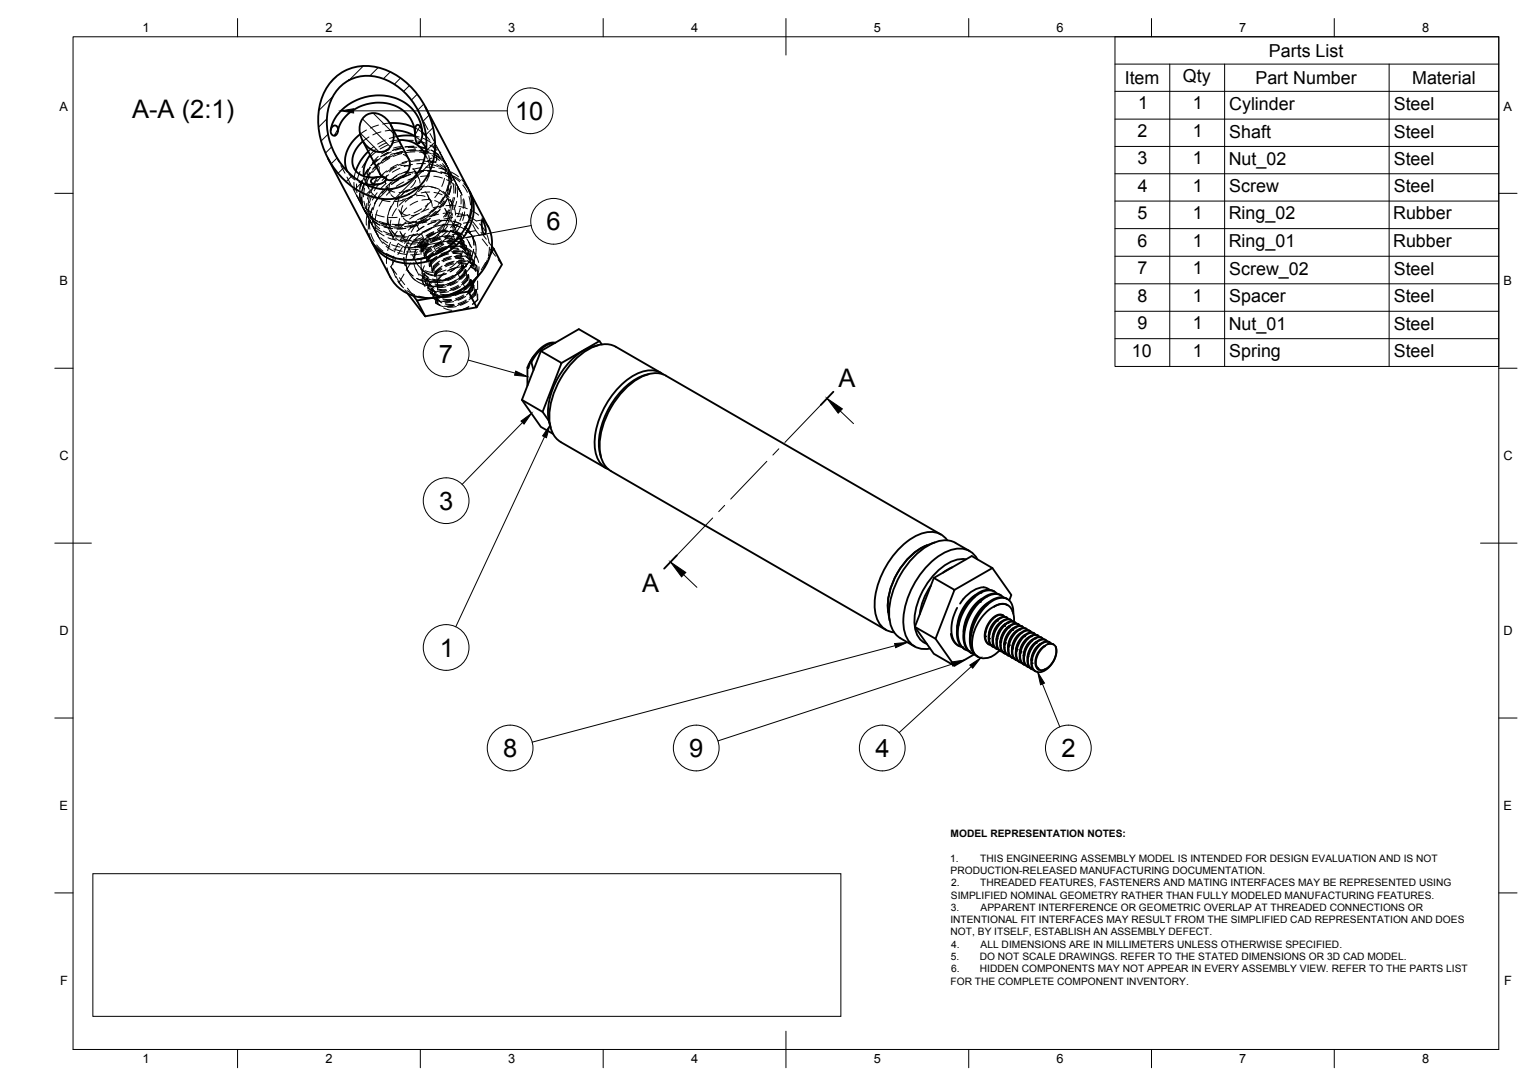
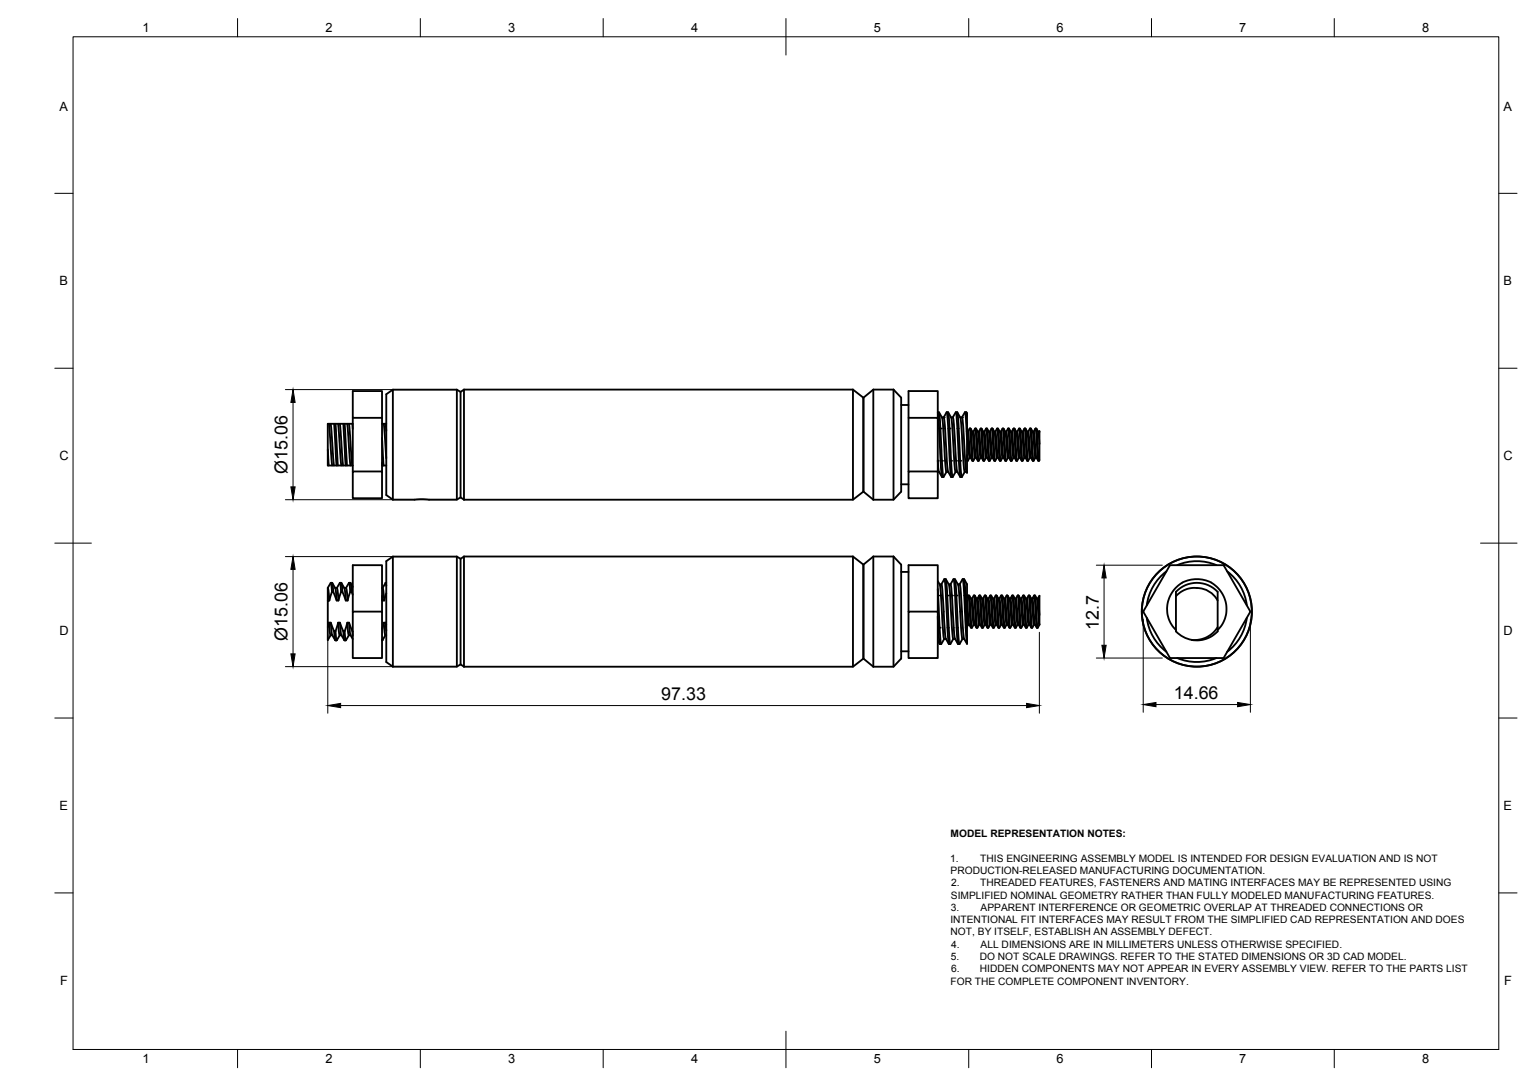
ISO-10303-21;
HEADER;
/* Generated by software containing ST-Developer
 * from STEP Tools, Inc. (www.steptools.com) 
 */

FILE_DESCRIPTION(
/* description */ (''),
/* implementation_level */ '2;1');

FILE_NAME(
/* name */ 'BR-313',
/* time_stamp */ '2026-10-06T13:05:37-07:00',
/* author */ (''),
/* organization */ (''),
/* preprocessor_version */ 'ST-DEVELOPER v20.2',
/* originating_system */ 'Autodesk Translation Framework v15.15.0.0',
/* authorisation */ '');

FILE_SCHEMA (('AUTOMOTIVE_DESIGN { 1 0 10303 214 3 1 1 }'));
ENDSEC;

DATA;
#10=MECHANICAL_DESIGN_GEOMETRIC_PRESENTATION_REPRESENTATION('',(#136,#137,
#138,#139,#140,#141,#142,#143,#144,#145),#28055);
#11=ITEM_DEFINED_TRANSFORMATION($,$,#3801,#4104);
#12=ITEM_DEFINED_TRANSFORMATION($,$,#3851,#4105);
#13=ITEM_DEFINED_TRANSFORMATION($,$,#3947,#4106);
#14=ITEM_DEFINED_TRANSFORMATION($,$,#3962,#4107);
#15=ITEM_DEFINED_TRANSFORMATION($,$,#3990,#4108);
#16=ITEM_DEFINED_TRANSFORMATION($,$,#4002,#4109);
#17=ITEM_DEFINED_TRANSFORMATION($,$,#4014,#4110);
#18=ITEM_DEFINED_TRANSFORMATION($,$,#4059,#4111);
#19=ITEM_DEFINED_TRANSFORMATION($,$,#4086,#4112);
#20=ITEM_DEFINED_TRANSFORMATION($,$,#4101,#4113);
#21=(
REPRESENTATION_RELATIONSHIP($,$,#28093,#28092)
REPRESENTATION_RELATIONSHIP_WITH_TRANSFORMATION(#11)
SHAPE_REPRESENTATION_RELATIONSHIP()
);
#22=(
REPRESENTATION_RELATIONSHIP($,$,#28094,#28092)
REPRESENTATION_RELATIONSHIP_WITH_TRANSFORMATION(#12)
SHAPE_REPRESENTATION_RELATIONSHIP()
);
#23=(
REPRESENTATION_RELATIONSHIP($,$,#28095,#28092)
REPRESENTATION_RELATIONSHIP_WITH_TRANSFORMATION(#13)
SHAPE_REPRESENTATION_RELATIONSHIP()
);
#24=(
REPRESENTATION_RELATIONSHIP($,$,#28096,#28092)
REPRESENTATION_RELATIONSHIP_WITH_TRANSFORMATION(#14)
SHAPE_REPRESENTATION_RELATIONSHIP()
);
#25=(
REPRESENTATION_RELATIONSHIP($,$,#28097,#28092)
REPRESENTATION_RELATIONSHIP_WITH_TRANSFORMATION(#15)
SHAPE_REPRESENTATION_RELATIONSHIP()
);
#26=(
REPRESENTATION_RELATIONSHIP($,$,#28098,#28092)
REPRESENTATION_RELATIONSHIP_WITH_TRANSFORMATION(#16)
SHAPE_REPRESENTATION_RELATIONSHIP()
);
#27=(
REPRESENTATION_RELATIONSHIP($,$,#28099,#28092)
REPRESENTATION_RELATIONSHIP_WITH_TRANSFORMATION(#17)
SHAPE_REPRESENTATION_RELATIONSHIP()
);
#28=(
REPRESENTATION_RELATIONSHIP($,$,#28100,#28092)
REPRESENTATION_RELATIONSHIP_WITH_TRANSFORMATION(#18)
SHAPE_REPRESENTATION_RELATIONSHIP()
);
#29=(
REPRESENTATION_RELATIONSHIP($,$,#28101,#28092)
REPRESENTATION_RELATIONSHIP_WITH_TRANSFORMATION(#19)
SHAPE_REPRESENTATION_RELATIONSHIP()
);
#30=(
REPRESENTATION_RELATIONSHIP($,$,#28102,#28092)
REPRESENTATION_RELATIONSHIP_WITH_TRANSFORMATION(#20)
SHAPE_REPRESENTATION_RELATIONSHIP()
);
#31=CONTEXT_DEPENDENT_SHAPE_REPRESENTATION(#21,#28082);
#32=CONTEXT_DEPENDENT_SHAPE_REPRESENTATION(#22,#28083);
#33=CONTEXT_DEPENDENT_SHAPE_REPRESENTATION(#23,#28084);
#34=CONTEXT_DEPENDENT_SHAPE_REPRESENTATION(#24,#28085);
#35=CONTEXT_DEPENDENT_SHAPE_REPRESENTATION(#25,#28086);
#36=CONTEXT_DEPENDENT_SHAPE_REPRESENTATION(#26,#28087);
#37=CONTEXT_DEPENDENT_SHAPE_REPRESENTATION(#27,#28088);
#38=CONTEXT_DEPENDENT_SHAPE_REPRESENTATION(#28,#28089);
#39=CONTEXT_DEPENDENT_SHAPE_REPRESENTATION(#29,#28090);
#40=CONTEXT_DEPENDENT_SHAPE_REPRESENTATION(#30,#28091);
#41=NEXT_ASSEMBLY_USAGE_OCCURRENCE('Cylinder:1','Cylinder:1',
'Cylinder:1',#28104,#28105,'Cylinder:1');
#42=NEXT_ASSEMBLY_USAGE_OCCURRENCE('Shaft:1','Shaft:1','Shaft:1',#28104,
#28106,'Shaft:1');
#43=NEXT_ASSEMBLY_USAGE_OCCURRENCE('Nut_02:1','Nut_02:1','Nut_02:1',#28104,
#28107,'Nut_02:1');
#44=NEXT_ASSEMBLY_USAGE_OCCURRENCE('Screw:1','Screw:1','Screw:1',#28104,
#28108,'Screw:1');
#45=NEXT_ASSEMBLY_USAGE_OCCURRENCE('Ring_02:1','Ring_02:1','Ring_02:1',
#28104,#28109,'Ring_02:1');
#46=NEXT_ASSEMBLY_USAGE_OCCURRENCE('Ring_01:1','Ring_01:1','Ring_01:1',
#28104,#28110,'Ring_01:1');
#47=NEXT_ASSEMBLY_USAGE_OCCURRENCE('Screw_02:1','Screw_02:1',
'Screw_02:1',#28104,#28111,'Screw_02:1');
#48=NEXT_ASSEMBLY_USAGE_OCCURRENCE('Spacer:1','Spacer:1','Spacer:1',#28104,
#28112,'Spacer:1');
#49=NEXT_ASSEMBLY_USAGE_OCCURRENCE('Nut_01:1','Nut_01:1','Nut_01:1',#28104,
#28113,'Nut_01:1');
#50=NEXT_ASSEMBLY_USAGE_OCCURRENCE('Spring:1','Spring:1','Spring:1',#28104,
#28114,'Spring:1');
#51=ORIENTED_CLOSED_SHELL('',*,#3684,.F.);
#52=ORIENTED_CLOSED_SHELL('',*,#3685,.F.);
#53=BREP_WITH_VOIDS('Body1',#3686,(#51,#52));
#54=ELLIPSE('',#4033,3.36109563026061,2.90329889035631);
#55=ELLIPSE('',#4034,2.84121050972126,2.43735261139454);
#56=ELLIPSE('',#4052,3.33206993022602,2.82346550068506);
#57=ELLIPSE('',#4053,2.87565474083181,2.48077736727696);
#58=B_SPLINE_SURFACE_WITH_KNOTS('',3,3,((#14364,#14365,#14366,#14367,#14368,
#14369,#14370,#14371,#14372,#14373,#14374,#14375,#14376,#14377,#14378,#14379,
#14380,#14381,#14382,#14383,#14384,#14385,#14386,#14387,#14388,#14389,#14390,
#14391,#14392,#14393,#14394,#14395,#14396,#14397,#14398,#14399,#14400,#14401,
#14402,#14403,#14404,#14405,#14406,#14407,#14408,#14409,#14410,#14411,#14412,
#14413,#14414,#14415,#14416,#14417,#14418,#14419,#14420,#14421,#14422,#14423,
#14424,#14425,#14426,#14427,#14428,#14429,#14430,#14431,#14432,#14433,#14434,
#14435,#14436,#14437,#14438,#14439,#14440,#14441,#14442,#14443,#14444,#14445,
#14446,#14447,#14448,#14449,#14450,#14451,#14452),(#14453,#14454,#14455,
#14456,#14457,#14458,#14459,#14460,#14461,#14462,#14463,#14464,#14465,#14466,
#14467,#14468,#14469,#14470,#14471,#14472,#14473,#14474,#14475,#14476,#14477,
#14478,#14479,#14480,#14481,#14482,#14483,#14484,#14485,#14486,#14487,#14488,
#14489,#14490,#14491,#14492,#14493,#14494,#14495,#14496,#14497,#14498,#14499,
#14500,#14501,#14502,#14503,#14504,#14505,#14506,#14507,#14508,#14509,#14510,
#14511,#14512,#14513,#14514,#14515,#14516,#14517,#14518,#14519,#14520,#14521,
#14522,#14523,#14524,#14525,#14526,#14527,#14528,#14529,#14530,#14531,#14532,
#14533,#14534,#14535,#14536,#14537,#14538,#14539,#14540,#14541),(#14542,
#14543,#14544,#14545,#14546,#14547,#14548,#14549,#14550,#14551,#14552,#14553,
#14554,#14555,#14556,#14557,#14558,#14559,#14560,#14561,#14562,#14563,#14564,
#14565,#14566,#14567,#14568,#14569,#14570,#14571,#14572,#14573,#14574,#14575,
#14576,#14577,#14578,#14579,#14580,#14581,#14582,#14583,#14584,#14585,#14586,
#14587,#14588,#14589,#14590,#14591,#14592,#14593,#14594,#14595,#14596,#14597,
#14598,#14599,#14600,#14601,#14602,#14603,#14604,#14605,#14606,#14607,#14608,
#14609,#14610,#14611,#14612,#14613,#14614,#14615,#14616,#14617,#14618,#14619,
#14620,#14621,#14622,#14623,#14624,#14625,#14626,#14627,#14628,#14629,#14630),
(#14631,#14632,#14633,#14634,#14635,#14636,#14637,#14638,#14639,#14640,
#14641,#14642,#14643,#14644,#14645,#14646,#14647,#14648,#14649,#14650,#14651,
#14652,#14653,#14654,#14655,#14656,#14657,#14658,#14659,#14660,#14661,#14662,
#14663,#14664,#14665,#14666,#14667,#14668,#14669,#14670,#14671,#14672,#14673,
#14674,#14675,#14676,#14677,#14678,#14679,#14680,#14681,#14682,#14683,#14684,
#14685,#14686,#14687,#14688,#14689,#14690,#14691,#14692,#14693,#14694,#14695,
#14696,#14697,#14698,#14699,#14700,#14701,#14702,#14703,#14704,#14705,#14706,
#14707,#14708,#14709,#14710,#14711,#14712,#14713,#14714,#14715,#14716,#14717,
#14718,#14719)),.UNSPECIFIED.,.F.,.F.,.F.,(4,4),(4,1,1,1,1,1,1,1,1,1,1,
1,1,1,1,1,1,1,1,1,1,1,1,1,1,1,1,1,1,1,1,1,1,1,1,1,1,1,1,1,1,1,1,1,1,1,1,
1,1,1,1,1,1,1,1,1,1,1,1,1,1,1,1,1,1,1,1,1,1,1,1,1,1,1,1,1,1,1,1,1,1,1,1,
1,1,1,4),(-0.000373179544599254,0.0497114942005783),(13.3942556087771,14.3924503130856,
15.3906450173941,16.3888397217026,17.3870344260111,18.3852291303196,19.3834238346281,
20.3816185389366,21.3798132432451,22.3780079475536,23.3762026518621,24.3743973561706,
25.3725920604791,26.3707867647876,27.3689814690961,28.3671761734046,29.365370877713,
30.3635655820215,31.36176028633,32.3599549906385,33.358149694947,34.3563443992555,
35.354539103564,36.3527338078725,37.350928512181,38.3491232164895,39.347317920798,
40.3455126251065,41.343707329415,42.3419020337235,43.340096738032,44.3382914423405,
45.336486146649,46.3346808509575,47.332875555266,48.3310702595745,49.329264963883,
50.3274596681915,51.3256543725,52.3238490768085,53.322043781117,54.3202384854255,
55.318433189734,56.3166278940425,57.314822598351,58.3130173026595,59.311212006968,
60.3094067112765,61.307601415585,62.3057961198935,63.303990824202,64.3021855285105,
65.300380232819,66.2985749371275,67.296769641436,68.2949643457444,69.2931590500529,
70.2913537543614,71.2895484586699,72.2877431629784,73.2859378672869,74.2841325715954,
75.2823272759039,76.2805219802124,77.2787166845209,78.2769113888294,79.2751060931379,
80.2733007974464,81.2714955017549,82.2696902060634,83.2678849103719,84.2660796146804,
85.2642743189889,86.2624690232974,87.2606637276059,88.2588584319144,89.2570531362229,
90.2552478405314,91.2534425448399,92.2516372491484,93.2498319534569,94.2480266577654,
95.2462213620739,96.2444160663824,97.2426107706909,98.2408054749994,99.2393733588525),
 .UNSPECIFIED.);
#59=B_SPLINE_SURFACE_WITH_KNOTS('',3,3,((#14976,#14977,#14978,#14979,#14980,
#14981,#14982,#14983,#14984,#14985,#14986,#14987,#14988,#14989,#14990,#14991,
#14992,#14993,#14994,#14995,#14996,#14997,#14998,#14999,#15000,#15001,#15002,
#15003,#15004,#15005,#15006,#15007,#15008,#15009,#15010,#15011,#15012,#15013,
#15014,#15015,#15016,#15017,#15018,#15019,#15020,#15021,#15022,#15023,#15024,
#15025,#15026,#15027,#15028,#15029,#15030,#15031,#15032,#15033,#15034,#15035,
#15036,#15037,#15038,#15039,#15040,#15041,#15042,#15043,#15044,#15045,#15046,
#15047,#15048,#15049,#15050,#15051,#15052,#15053,#15054,#15055,#15056,#15057,
#15058,#15059,#15060,#15061,#15062,#15063,#15064),(#15065,#15066,#15067,
#15068,#15069,#15070,#15071,#15072,#15073,#15074,#15075,#15076,#15077,#15078,
#15079,#15080,#15081,#15082,#15083,#15084,#15085,#15086,#15087,#15088,#15089,
#15090,#15091,#15092,#15093,#15094,#15095,#15096,#15097,#15098,#15099,#15100,
#15101,#15102,#15103,#15104,#15105,#15106,#15107,#15108,#15109,#15110,#15111,
#15112,#15113,#15114,#15115,#15116,#15117,#15118,#15119,#15120,#15121,#15122,
#15123,#15124,#15125,#15126,#15127,#15128,#15129,#15130,#15131,#15132,#15133,
#15134,#15135,#15136,#15137,#15138,#15139,#15140,#15141,#15142,#15143,#15144,
#15145,#15146,#15147,#15148,#15149,#15150,#15151,#15152,#15153),(#15154,
#15155,#15156,#15157,#15158,#15159,#15160,#15161,#15162,#15163,#15164,#15165,
#15166,#15167,#15168,#15169,#15170,#15171,#15172,#15173,#15174,#15175,#15176,
#15177,#15178,#15179,#15180,#15181,#15182,#15183,#15184,#15185,#15186,#15187,
#15188,#15189,#15190,#15191,#15192,#15193,#15194,#15195,#15196,#15197,#15198,
#15199,#15200,#15201,#15202,#15203,#15204,#15205,#15206,#15207,#15208,#15209,
#15210,#15211,#15212,#15213,#15214,#15215,#15216,#15217,#15218,#15219,#15220,
#15221,#15222,#15223,#15224,#15225,#15226,#15227,#15228,#15229,#15230,#15231,
#15232,#15233,#15234,#15235,#15236,#15237,#15238,#15239,#15240,#15241,#15242),
(#15243,#15244,#15245,#15246,#15247,#15248,#15249,#15250,#15251,#15252,
#15253,#15254,#15255,#15256,#15257,#15258,#15259,#15260,#15261,#15262,#15263,
#15264,#15265,#15266,#15267,#15268,#15269,#15270,#15271,#15272,#15273,#15274,
#15275,#15276,#15277,#15278,#15279,#15280,#15281,#15282,#15283,#15284,#15285,
#15286,#15287,#15288,#15289,#15290,#15291,#15292,#15293,#15294,#15295,#15296,
#15297,#15298,#15299,#15300,#15301,#15302,#15303,#15304,#15305,#15306,#15307,
#15308,#15309,#15310,#15311,#15312,#15313,#15314,#15315,#15316,#15317,#15318,
#15319,#15320,#15321,#15322,#15323,#15324,#15325,#15326,#15327,#15328,#15329,
#15330,#15331)),.UNSPECIFIED.,.F.,.F.,.F.,(4,4),(4,1,1,1,1,1,1,1,1,1,1,
1,1,1,1,1,1,1,1,1,1,1,1,1,1,1,1,1,1,1,1,1,1,1,1,1,1,1,1,1,1,1,1,1,1,1,1,
1,1,1,1,1,1,1,1,1,1,1,1,1,1,1,1,1,1,1,1,1,1,1,1,1,1,1,1,1,1,1,1,1,1,1,1,
1,1,1,4),(-0.000317322289268298,0.0497654761150975),(16.7016191235447,17.7001869884391,
18.6983816927476,19.6965763970561,20.6947711013646,21.6929658056731,22.6911605099816,
23.6893552142901,24.6875499185986,25.6857446229071,26.6839393272156,27.6821340315241,
28.6803287358326,29.6785234401411,30.6767181444496,31.6749128487581,32.6731075530666,
33.6713022573751,34.6694969616836,35.6676916659921,36.6658863703006,37.6640810746091,
38.6622757789176,39.6604704832261,40.6586651875346,41.6568598918431,42.6550545961516,
43.65324930046,44.6514440047685,45.6496387090771,46.6478334133855,47.646028117694,
48.6442228220025,49.642417526311,50.6406122306195,51.638806934928,52.6370016392365,
53.635196343545,54.6333910478535,55.631585752162,56.6297804564705,57.627975160779,
58.6261698650875,59.624364569396,60.6225592737045,61.620753978013,62.6189486823215,
63.61714338663,64.6153380909385,65.613532795247,66.6117274995555,67.609922203864,
68.6081169081725,69.606311612481,70.6045063167895,71.602701021098,72.6008957254065,
73.599090429715,74.5972851340235,75.595479838332,76.5936745426405,77.591869246949,
78.5900639512575,79.588258655566,80.5864533598745,81.584648064183,82.5828427684915,
83.5810374728,84.5792321771085,85.577426881417,86.5756215857255,87.573816290034,
88.5720109943425,89.570205698651,90.5684004029595,91.566595107268,92.5647898115765,
93.562984515885,94.5611792201935,95.559373924502,96.5575686288105,97.555763333119,
98.5539580374275,99.552152741736,100.550347446044,101.548542150353,102.546736854661),
 .UNSPECIFIED.);
#60=B_SPLINE_SURFACE_WITH_KNOTS('',3,1,((#15514,#15515),(#15516,#15517),
(#15518,#15519),(#15520,#15521),(#15522,#15523),(#15524,#15525),(#15526,
#15527),(#15528,#15529),(#15530,#15531),(#15532,#15533),(#15534,#15535),
(#15536,#15537),(#15538,#15539),(#15540,#15541)),.UNSPECIFIED.,.F.,.F.,
 .F.,(4,2,2,2,2,2,4),(2,2),(-0.844212290556731,-0.730966332817565,-0.619975754240938,
-0.457326579004558,-0.29977928179387,-0.147336283383114,0.),(0.,0.48),
 .UNSPECIFIED.);
#61=B_SPLINE_SURFACE_WITH_KNOTS('',3,1,((#15582,#15583),(#15584,#15585),
(#15586,#15587),(#15588,#15589),(#15590,#15591),(#15592,#15593),(#15594,
#15595),(#15596,#15597),(#15598,#15599),(#15600,#15601),(#15602,#15603),
(#15604,#15605),(#15606,#15607),(#15608,#15609)),.UNSPECIFIED.,.F.,.F.,
 .F.,(4,2,2,2,2,2,4),(2,2),(-0.847325527525843,-0.749719327139836,-0.649860858750851,
-0.495073659399383,-0.335166304629316,-0.170141007879843,0.),(0.,0.48),
 .UNSPECIFIED.);
#62=B_SPLINE_SURFACE_WITH_KNOTS('',3,3,((#20854,#20855,#20856,#20857,#20858,
#20859),(#20860,#20861,#20862,#20863,#20864,#20865),(#20866,#20867,#20868,
#20869,#20870,#20871),(#20872,#20873,#20874,#20875,#20876,#20877)),
 .UNSPECIFIED.,.F.,.F.,.F.,(4,4),(4,1,1,4),(0.,0.0494711118308268),(16.7019134878289,
17.6517088926312,18.6014255011318,19.5511421096324),.UNSPECIFIED.);
#63=B_SPLINE_SURFACE_WITH_KNOTS('',3,3,((#21117,#21118,#21119,#21120,#21121,
#21122),(#21123,#21124,#21125,#21126,#21127,#21128),(#21129,#21130,#21131,
#21132,#21133,#21134),(#21135,#21136,#21137,#21138,#21139,#21140)),
 .UNSPECIFIED.,.F.,.F.,.F.,(4,4),(4,1,1,4),(-7.87913040489834E-5,0.0493923155291723),
(13.3942556087771,14.3439722172777,15.2936888257783,16.2434842255829),
 .UNSPECIFIED.);
#64=B_SPLINE_SURFACE_WITH_KNOTS('',3,3,((#21329,#21330,#21331,#21332,#21333,
#21334,#21335,#21336,#21337,#21338,#21339,#21340,#21341,#21342,#21343,#21344,
#21345,#21346,#21347,#21348,#21349,#21350,#21351,#21352,#21353,#21354,#21355,
#21356,#21357,#21358,#21359,#21360,#21361,#21362,#21363,#21364,#21365,#21366,
#21367,#21368,#21369,#21370,#21371,#21372,#21373,#21374,#21375,#21376),
(#21377,#21378,#21379,#21380,#21381,#21382,#21383,#21384,#21385,#21386,
#21387,#21388,#21389,#21390,#21391,#21392,#21393,#21394,#21395,#21396,#21397,
#21398,#21399,#21400,#21401,#21402,#21403,#21404,#21405,#21406,#21407,#21408,
#21409,#21410,#21411,#21412,#21413,#21414,#21415,#21416,#21417,#21418,#21419,
#21420,#21421,#21422,#21423,#21424),(#21425,#21426,#21427,#21428,#21429,
#21430,#21431,#21432,#21433,#21434,#21435,#21436,#21437,#21438,#21439,#21440,
#21441,#21442,#21443,#21444,#21445,#21446,#21447,#21448,#21449,#21450,#21451,
#21452,#21453,#21454,#21455,#21456,#21457,#21458,#21459,#21460,#21461,#21462,
#21463,#21464,#21465,#21466,#21467,#21468,#21469,#21470,#21471,#21472),
(#21473,#21474,#21475,#21476,#21477,#21478,#21479,#21480,#21481,#21482,
#21483,#21484,#21485,#21486,#21487,#21488,#21489,#21490,#21491,#21492,#21493,
#21494,#21495,#21496,#21497,#21498,#21499,#21500,#21501,#21502,#21503,#21504,
#21505,#21506,#21507,#21508,#21509,#21510,#21511,#21512,#21513,#21514,#21515,
#21516,#21517,#21518,#21519,#21520)),.UNSPECIFIED.,.F.,.F.,.F.,(4,4),(4,
1,1,1,1,1,1,1,1,1,1,1,1,1,1,1,1,1,1,1,1,1,1,1,1,1,1,1,1,1,1,1,1,1,1,1,1,
1,1,1,1,1,1,1,1,4),(-0.000683464176930082,0.0823722747458684),(8.31487785380719,
8.80643119756841,9.29798454132964,10.2810912288521,11.2641979163745,12.247304603897,
13.2304112914194,14.2135179789419,15.1966246664643,16.1797313539867,17.1628380415092,
18.1459447290316,19.1290514165541,20.1121581040765,21.095264791599,22.0783714791214,
23.0614781666439,24.0445848541663,25.0276915416888,26.0107982292112,26.9939049167336,
27.9770116042561,28.9601182917785,29.943224979301,30.9263316668234,31.9094383543459,
32.8925450418683,33.8756517293908,34.8587584169132,35.8418651044356,36.8249717919581,
37.8080784794805,38.791185167003,39.7742918545254,40.7573985420479,41.7405052295703,
42.7236119170928,43.7067186046152,44.6898252921376,45.6729319796601,46.6560386671825,
47.639145354705,48.6222520422274,49.6053587297499,50.0969120735111,50.5891488814492),
 .UNSPECIFIED.);
#65=B_SPLINE_SURFACE_WITH_KNOTS('',3,3,((#21721,#21722,#21723,#21724,#21725,
#21726,#21727,#21728,#21729,#21730,#21731,#21732,#21733,#21734,#21735,#21736,
#21737,#21738,#21739,#21740,#21741,#21742,#21743,#21744,#21745,#21746,#21747,
#21748,#21749,#21750,#21751,#21752,#21753,#21754,#21755,#21756,#21757,#21758,
#21759,#21760,#21761,#21762,#21763,#21764,#21765,#21766,#21767,#21768),
(#21769,#21770,#21771,#21772,#21773,#21774,#21775,#21776,#21777,#21778,
#21779,#21780,#21781,#21782,#21783,#21784,#21785,#21786,#21787,#21788,#21789,
#21790,#21791,#21792,#21793,#21794,#21795,#21796,#21797,#21798,#21799,#21800,
#21801,#21802,#21803,#21804,#21805,#21806,#21807,#21808,#21809,#21810,#21811,
#21812,#21813,#21814,#21815,#21816),(#21817,#21818,#21819,#21820,#21821,
#21822,#21823,#21824,#21825,#21826,#21827,#21828,#21829,#21830,#21831,#21832,
#21833,#21834,#21835,#21836,#21837,#21838,#21839,#21840,#21841,#21842,#21843,
#21844,#21845,#21846,#21847,#21848,#21849,#21850,#21851,#21852,#21853,#21854,
#21855,#21856,#21857,#21858,#21859,#21860,#21861,#21862,#21863,#21864),
(#21865,#21866,#21867,#21868,#21869,#21870,#21871,#21872,#21873,#21874,
#21875,#21876,#21877,#21878,#21879,#21880,#21881,#21882,#21883,#21884,#21885,
#21886,#21887,#21888,#21889,#21890,#21891,#21892,#21893,#21894,#21895,#21896,
#21897,#21898,#21899,#21900,#21901,#21902,#21903,#21904,#21905,#21906,#21907,
#21908,#21909,#21910,#21911,#21912)),.UNSPECIFIED.,.F.,.F.,.F.,(4,4),(4,
1,1,1,1,1,1,1,1,1,1,1,1,1,1,1,1,1,1,1,1,1,1,1,1,1,1,1,1,1,1,1,1,1,1,1,1,
1,1,1,1,1,1,1,1,4),(-0.000359643560771195,0.0826961570524529),(11.6143855724915,
12.1066224675668,12.598175811328,13.5812824988505,14.5643891863729,15.5474958738954,
16.5306025614178,17.5137092489403,18.4968159364627,19.4799226239851,20.4630293115076,
21.44613599903,22.4292426865525,23.4123493740749,24.3954560615974,25.3785627491198,
26.3616694366423,27.3447761241647,28.3278828116872,29.3109894992096,30.294096186732,
31.2772028742545,32.2603095617769,33.2434162492994,34.2265229368218,35.2096296243443,
36.1927363118667,37.1758429993892,38.1589496869116,39.142056374434,40.1251630619565,
41.1082697494789,42.0913764370014,43.0744831245238,44.0575898120463,45.0406964995687,
46.0238031870912,47.0069098746136,47.9900165621361,48.9731232496585,49.956229937181,
50.9393366247034,51.9224433122258,52.9055499997483,53.3971033435095,53.8886566872707),
 .UNSPECIFIED.);
#66=B_SPLINE_SURFACE_WITH_KNOTS('',3,3,((#24618,#24619,#24620,#24621),(#24622,
#24623,#24624,#24625),(#24626,#24627,#24628,#24629),(#24630,#24631,#24632,
#24633)),.UNSPECIFIED.,.F.,.F.,.F.,(4,4),(4,4),(0.066620174713851,0.0820126057383863),
(8.314732749858,8.70158673567856),.UNSPECIFIED.);
#67=B_SPLINE_SURFACE_WITH_KNOTS('',3,3,((#24640,#24641,#24642,#24643,#24644,
#24645),(#24646,#24647,#24648,#24649,#24650,#24651),(#24652,#24653,#24654,
#24655,#24656,#24657),(#24658,#24659,#24660,#24661,#24662,#24663)),
 .UNSPECIFIED.,.F.,.F.,.F.,(4,4),(4,1,1,4),(-0.000175214539722031,0.0820126057383863),
(47.6103505270742,48.3332993342991,49.0560729269844,49.7790217342094),
 .UNSPECIFIED.);
#68=B_SPLINE_SURFACE_WITH_KNOTS('',3,3,((#24719,#24720,#24721,#24722,#24723,
#24724),(#24725,#24726,#24727,#24728,#24729,#24730),(#24731,#24732,#24733,
#24734,#24735,#24736),(#24737,#24738,#24739,#24740,#24741,#24742)),
 .UNSPECIFIED.,.F.,.F.,.F.,(4,4),(4,1,1,4),(-0.000176040298938268,0.0820126057383863),
(41.3271643941354,42.0501140271196,42.7728876198048,43.495837252789),
 .UNSPECIFIED.);
#69=B_SPLINE_SURFACE_WITH_KNOTS('',3,3,((#24749,#24750,#24751,#24752,#24753,
#24754),(#24755,#24756,#24757,#24758,#24759,#24760),(#24761,#24762,#24763,
#24764,#24765,#24766),(#24767,#24768,#24769,#24770,#24771,#24772)),
 .UNSPECIFIED.,.F.,.F.,.F.,(4,4),(4,1,1,4),(-0.000176780710812022,0.0820126057383863),
(35.0439783465439,35.76692871994,36.4897023126252,37.2126526860213),
 .UNSPECIFIED.);
#70=B_SPLINE_SURFACE_WITH_KNOTS('',3,3,((#24779,#24780,#24781,#24782,#24783,
#24784),(#24785,#24786,#24787,#24788,#24789,#24790),(#24791,#24792,#24793,
#24794,#24795,#24796),(#24797,#24798,#24799,#24800,#24801,#24802)),
 .UNSPECIFIED.,.F.,.F.,.F.,(4,4),(4,1,1,4),(-0.000177449278394063,0.0820126057383863),
(28.7607923707967,29.4837434127604,30.2065170054456,30.9294680474093),
 .UNSPECIFIED.);
#71=B_SPLINE_SURFACE_WITH_KNOTS('',3,3,((#24809,#24810,#24811,#24812,#24813,
#24814),(#24815,#24816,#24817,#24818,#24819,#24820),(#24821,#24822,#24823,
#24824,#24825,#24826),(#24827,#24828,#24829,#24830,#24831,#24832)),
 .UNSPECIFIED.,.F.,.F.,.F.,(4,4),(4,1,1,4),(-0.000178056708344039,0.0820126057383863),
(22.4776064561872,23.2005581055808,23.9233316982661,24.6462833476596),
 .UNSPECIFIED.);
#72=B_SPLINE_SURFACE_WITH_KNOTS('',3,3,((#24839,#24840,#24841,#24842,#24843,
#24844),(#24845,#24846,#24847,#24848,#24849,#24850),(#24851,#24852,#24853,
#24854,#24855,#24856),(#24857,#24858,#24859,#24860,#24861,#24862)),
 .UNSPECIFIED.,.F.,.F.,.F.,(4,4),(4,1,1,4),(-0.000178611609329685,0.0820126057383863),
(16.1944205941067,16.9173727984012,17.6401463910865,18.363098595381),
 .UNSPECIFIED.);
#73=B_SPLINE_SURFACE_WITH_KNOTS('',3,3,((#24869,#24870,#24871,#24872,#24873,
#24874),(#24875,#24876,#24877,#24878,#24879,#24880),(#24881,#24882,#24883,
#24884,#24885,#24886),(#24887,#24888,#24889,#24890,#24891,#24892)),
 .UNSPECIFIED.,.F.,.F.,.F.,(4,4),(4,1,1,4),(-0.000156396744294902,0.0821188966323171),
(9.98287940740301,10.6818311637994,11.3807829201958,12.0798910733364),
 .UNSPECIFIED.);
#74=B_SPLINE_SURFACE_WITH_KNOTS('',3,3,((#24952,#24953,#24954,#24955,#24956,
#24957),(#24958,#24959,#24960,#24961,#24962,#24963),(#24964,#24965,#24966,
#24967,#24968,#24969),(#24970,#24971,#24972,#24973,#24974,#24975)),
 .UNSPECIFIED.,.F.,.F.,.F.,(4,4),(4,1,1,4),(-0.000175639065612779,0.0820126057383863),
(44.4687574489585,45.1917066807094,45.9144802733946,46.6374295051455),
 .UNSPECIFIED.);
#75=B_SPLINE_SURFACE_WITH_KNOTS('',3,3,((#24982,#24983,#24984,#24985,#24986,
#24987),(#24988,#24989,#24990,#24991,#24992,#24993),(#24994,#24995,#24996,
#24997,#24998,#24999),(#25000,#25001,#25002,#25003,#25004,#25005)),
 .UNSPECIFIED.,.F.,.F.,.F.,(4,4),(4,1,1,4),(-0.000176420253877423,0.0820126057383863),
(38.1855713605906,38.9085213735298,39.631294966215,40.3542449791542),
 .UNSPECIFIED.);
#76=B_SPLINE_SURFACE_WITH_KNOTS('',3,3,((#25012,#25013,#25014,#25015,#25016,
#25017),(#25018,#25019,#25020,#25021,#25022,#25023),(#25024,#25025,#25026,
#25027,#25028,#25029),(#25030,#25031,#25032,#25033,#25034,#25035)),
 .UNSPECIFIED.,.F.,.F.,.F.,(4,4),(4,1,1,4),(-0.000177123249794933,0.0820126057383863),
(31.9023853504151,32.6253360663502,33.3481096590354,34.0710603749705),
 .UNSPECIFIED.);
#77=B_SPLINE_SURFACE_WITH_KNOTS('',3,3,((#25042,#25043,#25044,#25045,#25046,
#25047),(#25048,#25049,#25050,#25051,#25052,#25053),(#25054,#25055,#25056,
#25057,#25058,#25059),(#25060,#25061,#25062,#25063,#25064,#25065)),
 .UNSPECIFIED.,.F.,.F.,.F.,(4,4),(4,1,1,4),(-0.000177760054985351,0.0820126057383863),
(25.6191994064303,26.3421507591706,27.0649243518558,27.7878757045961),
 .UNSPECIFIED.);
#78=B_SPLINE_SURFACE_WITH_KNOTS('',3,3,((#25072,#25073,#25074,#25075,#25076,
#25077),(#25078,#25079,#25080,#25081,#25082,#25083),(#25084,#25085,#25086,
#25087,#25088,#25089),(#25090,#25091,#25092,#25093,#25094,#25095)),
 .UNSPECIFIED.,.F.,.F.,.F.,(4,4),(4,1,1,4),(-0.000178340254205606,0.0820126057383863),
(19.3360135190516,20.058965451991,20.7817390446763,21.5046909776157),
 .UNSPECIFIED.);
#79=B_SPLINE_SURFACE_WITH_KNOTS('',3,3,((#25102,#25103,#25104,#25105,#25106,
#25107),(#25108,#25109,#25110,#25111,#25112,#25113),(#25114,#25115,#25116,
#25117,#25118,#25119),(#25120,#25121,#25122,#25123,#25124,#25125)),
 .UNSPECIFIED.,.F.,.F.,.F.,(4,4),(4,1,1,4),(-0.000178871603495943,0.0820126057383863),
(13.0528276805227,13.7757801448114,14.4985537374967,15.2215062017854),
 .UNSPECIFIED.);
#80=B_SPLINE_SURFACE_WITH_KNOTS('',3,3,((#25323,#25324,#25325,#25326,#25327,
#25328),(#25329,#25330,#25331,#25332,#25333,#25334),(#25335,#25336,#25337,
#25338,#25339,#25340),(#25341,#25342,#25343,#25344,#25345,#25346)),
 .UNSPECIFIED.,.F.,.F.,.F.,(4,4),(4,1,1,4),(0.,0.0821885306368104),(47.6103498167155,
48.3332993342991,49.0560729269844,49.7790224445681),.UNSPECIFIED.);
#81=B_SPLINE_SURFACE_WITH_KNOTS('',3,3,((#25347,#25348,#25349,#25350,#25351,
#25352),(#25353,#25354,#25355,#25356,#25357,#25358),(#25359,#25360,#25361,
#25362,#25363,#25364),(#25365,#25366,#25367,#25368,#25369,#25370)),
 .UNSPECIFIED.,.F.,.F.,.F.,(4,4),(4,1,1,4),(0.,0.0821892826429367),(41.3271637575297,
42.0501140271195,42.7728876198048,43.4958378893947),.UNSPECIFIED.);
#82=B_SPLINE_SURFACE_WITH_KNOTS('',3,3,((#25371,#25372,#25373,#25374,#25375,
#25376),(#25377,#25378,#25379,#25380,#25381,#25382),(#25383,#25384,#25385,
#25386,#25387,#25388),(#25389,#25390,#25391,#25392,#25393,#25394)),
 .UNSPECIFIED.,.F.,.F.,.F.,(4,4),(4,1,1,4),(0.,0.0821899610193562),(35.0439777719737,
35.76692871994,36.4897023126252,37.2126532605915),.UNSPECIFIED.);
#83=B_SPLINE_SURFACE_WITH_KNOTS('',3,3,((#25395,#25396,#25397,#25398,#25399,
#25400),(#25401,#25402,#25403,#25404,#25405,#25406),(#25407,#25408,#25409,
#25410,#25411,#25412),(#25413,#25414,#25415,#25416,#25417,#25418)),
 .UNSPECIFIED.,.F.,.F.,.F.,(4,4),(4,1,1,4),(0.,0.0821905768332721),(28.7607918489802,
29.4837434127604,30.2065170054456,30.9294685692258),.UNSPECIFIED.);
#84=B_SPLINE_SURFACE_WITH_KNOTS('',3,3,((#25419,#25420,#25421,#25422,#25423,
#25424),(#25425,#25426,#25427,#25428,#25429,#25430),(#25431,#25432,#25433,
#25434,#25435,#25436),(#25437,#25438,#25439,#25440,#25441,#25442)),
 .UNSPECIFIED.,.F.,.F.,.F.,(4,4),(4,1,1,4),(0.,0.0821911389659494),(22.4776059796679,
23.2005581055808,23.9233316982661,24.6462838241789),.UNSPECIFIED.);
#85=B_SPLINE_SURFACE_WITH_KNOTS('',3,3,((#25443,#25444,#25445,#25446,#25447,
#25448),(#25449,#25450,#25451,#25452,#25453,#25454),(#25455,#25456,#25457,
#25458,#25459,#25460),(#25461,#25462,#25463,#25464,#25465,#25466)),
 .UNSPECIFIED.,.F.,.F.,.F.,(4,4),(4,1,1,4),(0.,0.0821916546351816),(16.1944201568192,
16.9173727984012,17.6401463910865,18.3630990326685),.UNSPECIFIED.);
#86=B_SPLINE_SURFACE_WITH_KNOTS('',3,3,((#25467,#25468,#25469,#25470,#25471,
#25472),(#25473,#25474,#25475,#25476,#25477,#25478),(#25479,#25480,#25481,
#25482,#25483,#25484),(#25485,#25486,#25487,#25488,#25489,#25490)),
 .UNSPECIFIED.,.F.,.F.,.F.,(4,4),(4,1,1,4),(-9.65518509377315E-5,0.0821438972802576),
(50.7519871036618,51.4243296588263,52.0965409224489,52.7687521860715),
 .UNSPECIFIED.);
#87=B_SPLINE_SURFACE_WITH_KNOTS('',3,3,((#25491,#25492,#25493,#25494,#25495,
#25496),(#25497,#25498,#25499,#25500,#25501,#25502),(#25503,#25504,#25505,
#25506,#25507,#25508),(#25509,#25510,#25511,#25512,#25513,#25514)),
 .UNSPECIFIED.,.F.,.F.,.F.,(4,4),(4,1,1,4),(0.,0.08218891663892),(44.4687567771236,
45.1917066807094,45.9144802733946,46.6374301769804),.UNSPECIFIED.);
#88=B_SPLINE_SURFACE_WITH_KNOTS('',3,3,((#25515,#25516,#25517,#25518,#25519,
#25520),(#25521,#25522,#25523,#25524,#25525,#25526),(#25527,#25528,#25529,
#25530,#25531,#25532),(#25533,#25534,#25535,#25536,#25537,#25538)),
 .UNSPECIFIED.,.F.,.F.,.F.,(4,4),(4,1,1,4),(0.,0.0821896302845616),(38.1855707562983,
38.9085213735298,39.631294966215,40.3542455834465),.UNSPECIFIED.);
#89=B_SPLINE_SURFACE_WITH_KNOTS('',3,3,((#25539,#25540,#25541,#25542,#25543,
#25544),(#25545,#25546,#25547,#25548,#25549,#25550),(#25551,#25552,#25553,
#25554,#25555,#25556),(#25557,#25558,#25559,#25560,#25561,#25562)),
 .UNSPECIFIED.,.F.,.F.,.F.,(4,4),(4,1,1,4),(0.,0.0821902761472763),(31.902384803256,
32.6253360663502,33.3481096590354,34.0710609221296),.UNSPECIFIED.);
#90=B_SPLINE_SURFACE_WITH_KNOTS('',3,3,((#25563,#25564,#25565,#25566,#25567,
#25568),(#25569,#25570,#25571,#25572,#25573,#25574),(#25575,#25576,#25577,
#25578,#25579,#25580),(#25581,#25582,#25583,#25584,#25585,#25586)),
 .UNSPECIFIED.,.F.,.F.,.F.,(4,4),(4,1,1,4),(0.,0.0821908641246751),(25.619198908099,
26.3421507591706,27.0649243518559,27.7878762029274),.UNSPECIFIED.);
#91=B_SPLINE_SURFACE_WITH_KNOTS('',3,3,((#25587,#25588,#25589,#25590,#25591,
#25592),(#25593,#25594,#25595,#25596,#25597,#25598),(#25599,#25600,#25601,
#25602,#25603,#25604),(#25605,#25606,#25607,#25608,#25609,#25610)),
 .UNSPECIFIED.,.F.,.F.,.F.,(4,4),(4,1,1,4),(0.,0.0821914022112513),(19.3360130628329,
20.058965451991,20.7817390446763,21.5046914338344),.UNSPECIFIED.);
#92=B_SPLINE_SURFACE_WITH_KNOTS('',3,3,((#25611,#25612,#25613,#25614,#25615,
#25616),(#25617,#25618,#25619,#25620,#25621,#25622),(#25623,#25624,#25625,
#25626,#25627,#25628),(#25629,#25630,#25631,#25632,#25633,#25634)),
 .UNSPECIFIED.,.F.,.F.,.F.,(4,4),(4,1,1,4),(0.,0.0821918969420234),(13.0528272609226,
13.7757801448114,14.4985537374967,15.2215066213855),.UNSPECIFIED.);
#93=B_SPLINE_SURFACE_WITH_KNOTS('',3,3,((#25636,#25637,#25638,#25639),(#25640,
#25641,#25642,#25643),(#25644,#25645,#25646,#25647),(#25648,#25649,#25650,
#25651)),.UNSPECIFIED.,.F.,.F.,.F.,(4,4),(4,4),(0.0663734465876268,0.0820126057383863),
(11.6152142277547,12.0797346765921),.UNSPECIFIED.);
#94=B_SPLINE_SURFACE_WITH_KNOTS('',3,1,((#25707,#25708),(#25709,#25710),
(#25711,#25712),(#25713,#25714),(#25715,#25716),(#25717,#25718),(#25719,
#25720),(#25721,#25722),(#25723,#25724),(#25725,#25726),(#25727,#25728),
(#25729,#25730),(#25731,#25732),(#25733,#25734)),.UNSPECIFIED.,.F.,.F.,
 .F.,(4,2,2,2,2,2,4),(2,2),(-0.844212290556731,-0.730966332817565,-0.619975754240938,
-0.457326579004558,-0.29977928179387,-0.147336283383114,0.),(0.,0.48),
 .UNSPECIFIED.);
#95=B_SPLINE_SURFACE_WITH_KNOTS('',3,1,((#25775,#25776),(#25777,#25778),
(#25779,#25780),(#25781,#25782),(#25783,#25784),(#25785,#25786),(#25787,
#25788),(#25789,#25790),(#25791,#25792),(#25793,#25794),(#25795,#25796),
(#25797,#25798),(#25799,#25800),(#25801,#25802)),.UNSPECIFIED.,.F.,.F.,
 .F.,(4,2,2,2,2,2,4),(2,2),(-0.847325527525843,-0.749719327139836,-0.649860858750851,
-0.495073659399383,-0.335166304629316,-0.170141007879843,0.),(0.,0.48),
 .UNSPECIFIED.);
#96=B_SPLINE_SURFACE_WITH_KNOTS('',3,3,((#25876,#25877,#25878,#25879,#25880,
#25881,#25882,#25883,#25884,#25885,#25886,#25887,#25888,#25889,#25890,#25891,
#25892,#25893,#25894,#25895,#25896,#25897,#25898,#25899,#25900,#25901,#25902,
#25903,#25904,#25905,#25906,#25907,#25908,#25909,#25910,#25911,#25912,#25913,
#25914,#25915,#25916,#25917,#25918,#25919,#25920,#25921,#25922,#25923,#25924,
#25925,#25926,#25927,#25928,#25929,#25930,#25931,#25932,#25933,#25934,#25935,
#25936,#25937,#25938,#25939,#25940,#25941,#25942,#25943,#25944,#25945,#25946,
#25947,#25948,#25949,#25950,#25951,#25952,#25953,#25954),(#25955,#25956,
#25957,#25958,#25959,#25960,#25961,#25962,#25963,#25964,#25965,#25966,#25967,
#25968,#25969,#25970,#25971,#25972,#25973,#25974,#25975,#25976,#25977,#25978,
#25979,#25980,#25981,#25982,#25983,#25984,#25985,#25986,#25987,#25988,#25989,
#25990,#25991,#25992,#25993,#25994,#25995,#25996,#25997,#25998,#25999,#26000,
#26001,#26002,#26003,#26004,#26005,#26006,#26007,#26008,#26009,#26010,#26011,
#26012,#26013,#26014,#26015,#26016,#26017,#26018,#26019,#26020,#26021,#26022,
#26023,#26024,#26025,#26026,#26027,#26028,#26029,#26030,#26031,#26032,#26033),
(#26034,#26035,#26036,#26037,#26038,#26039,#26040,#26041,#26042,#26043,
#26044,#26045,#26046,#26047,#26048,#26049,#26050,#26051,#26052,#26053,#26054,
#26055,#26056,#26057,#26058,#26059,#26060,#26061,#26062,#26063,#26064,#26065,
#26066,#26067,#26068,#26069,#26070,#26071,#26072,#26073,#26074,#26075,#26076,
#26077,#26078,#26079,#26080,#26081,#26082,#26083,#26084,#26085,#26086,#26087,
#26088,#26089,#26090,#26091,#26092,#26093,#26094,#26095,#26096,#26097,#26098,
#26099,#26100,#26101,#26102,#26103,#26104,#26105,#26106,#26107,#26108,#26109,
#26110,#26111,#26112),(#26113,#26114,#26115,#26116,#26117,#26118,#26119,
#26120,#26121,#26122,#26123,#26124,#26125,#26126,#26127,#26128,#26129,#26130,
#26131,#26132,#26133,#26134,#26135,#26136,#26137,#26138,#26139,#26140,#26141,
#26142,#26143,#26144,#26145,#26146,#26147,#26148,#26149,#26150,#26151,#26152,
#26153,#26154,#26155,#26156,#26157,#26158,#26159,#26160,#26161,#26162,#26163,
#26164,#26165,#26166,#26167,#26168,#26169,#26170,#26171,#26172,#26173,#26174,
#26175,#26176,#26177,#26178,#26179,#26180,#26181,#26182,#26183,#26184,#26185,
#26186,#26187,#26188,#26189,#26190,#26191),(#26192,#26193,#26194,#26195,
#26196,#26197,#26198,#26199,#26200,#26201,#26202,#26203,#26204,#26205,#26206,
#26207,#26208,#26209,#26210,#26211,#26212,#26213,#26214,#26215,#26216,#26217,
#26218,#26219,#26220,#26221,#26222,#26223,#26224,#26225,#26226,#26227,#26228,
#26229,#26230,#26231,#26232,#26233,#26234,#26235,#26236,#26237,#26238,#26239,
#26240,#26241,#26242,#26243,#26244,#26245,#26246,#26247,#26248,#26249,#26250,
#26251,#26252,#26253,#26254,#26255,#26256,#26257,#26258,#26259,#26260,#26261,
#26262,#26263,#26264,#26265,#26266,#26267,#26268,#26269,#26270),(#26271,
#26272,#26273,#26274,#26275,#26276,#26277,#26278,#26279,#26280,#26281,#26282,
#26283,#26284,#26285,#26286,#26287,#26288,#26289,#26290,#26291,#26292,#26293,
#26294,#26295,#26296,#26297,#26298,#26299,#26300,#26301,#26302,#26303,#26304,
#26305,#26306,#26307,#26308,#26309,#26310,#26311,#26312,#26313,#26314,#26315,
#26316,#26317,#26318,#26319,#26320,#26321,#26322,#26323,#26324,#26325,#26326,
#26327,#26328,#26329,#26330,#26331,#26332,#26333,#26334,#26335,#26336,#26337,
#26338,#26339,#26340,#26341,#26342,#26343,#26344,#26345,#26346,#26347,#26348,
#26349),(#26350,#26351,#26352,#26353,#26354,#26355,#26356,#26357,#26358,
#26359,#26360,#26361,#26362,#26363,#26364,#26365,#26366,#26367,#26368,#26369,
#26370,#26371,#26372,#26373,#26374,#26375,#26376,#26377,#26378,#26379,#26380,
#26381,#26382,#26383,#26384,#26385,#26386,#26387,#26388,#26389,#26390,#26391,
#26392,#26393,#26394,#26395,#26396,#26397,#26398,#26399,#26400,#26401,#26402,
#26403,#26404,#26405,#26406,#26407,#26408,#26409,#26410,#26411,#26412,#26413,
#26414,#26415,#26416,#26417,#26418,#26419,#26420,#26421,#26422,#26423,#26424,
#26425,#26426,#26427,#26428),(#26429,#26430,#26431,#26432,#26433,#26434,
#26435,#26436,#26437,#26438,#26439,#26440,#26441,#26442,#26443,#26444,#26445,
#26446,#26447,#26448,#26449,#26450,#26451,#26452,#26453,#26454,#26455,#26456,
#26457,#26458,#26459,#26460,#26461,#26462,#26463,#26464,#26465,#26466,#26467,
#26468,#26469,#26470,#26471,#26472,#26473,#26474,#26475,#26476,#26477,#26478,
#26479,#26480,#26481,#26482,#26483,#26484,#26485,#26486,#26487,#26488,#26489,
#26490,#26491,#26492,#26493,#26494,#26495,#26496,#26497,#26498,#26499,#26500,
#26501,#26502,#26503,#26504,#26505,#26506,#26507),(#26508,#26509,#26510,
#26511,#26512,#26513,#26514,#26515,#26516,#26517,#26518,#26519,#26520,#26521,
#26522,#26523,#26524,#26525,#26526,#26527,#26528,#26529,#26530,#26531,#26532,
#26533,#26534,#26535,#26536,#26537,#26538,#26539,#26540,#26541,#26542,#26543,
#26544,#26545,#26546,#26547,#26548,#26549,#26550,#26551,#26552,#26553,#26554,
#26555,#26556,#26557,#26558,#26559,#26560,#26561,#26562,#26563,#26564,#26565,
#26566,#26567,#26568,#26569,#26570,#26571,#26572,#26573,#26574,#26575,#26576,
#26577,#26578,#26579,#26580,#26581,#26582,#26583,#26584,#26585,#26586),
(#26587,#26588,#26589,#26590,#26591,#26592,#26593,#26594,#26595,#26596,
#26597,#26598,#26599,#26600,#26601,#26602,#26603,#26604,#26605,#26606,#26607,
#26608,#26609,#26610,#26611,#26612,#26613,#26614,#26615,#26616,#26617,#26618,
#26619,#26620,#26621,#26622,#26623,#26624,#26625,#26626,#26627,#26628,#26629,
#26630,#26631,#26632,#26633,#26634,#26635,#26636,#26637,#26638,#26639,#26640,
#26641,#26642,#26643,#26644,#26645,#26646,#26647,#26648,#26649,#26650,#26651,
#26652,#26653,#26654,#26655,#26656,#26657,#26658,#26659,#26660,#26661,#26662,
#26663,#26664,#26665),(#26666,#26667,#26668,#26669,#26670,#26671,#26672,
#26673,#26674,#26675,#26676,#26677,#26678,#26679,#26680,#26681,#26682,#26683,
#26684,#26685,#26686,#26687,#26688,#26689,#26690,#26691,#26692,#26693,#26694,
#26695,#26696,#26697,#26698,#26699,#26700,#26701,#26702,#26703,#26704,#26705,
#26706,#26707,#26708,#26709,#26710,#26711,#26712,#26713,#26714,#26715,#26716,
#26717,#26718,#26719,#26720,#26721,#26722,#26723,#26724,#26725,#26726,#26727,
#26728,#26729,#26730,#26731,#26732,#26733,#26734,#26735,#26736,#26737,#26738,
#26739,#26740,#26741,#26742,#26743,#26744),(#26745,#26746,#26747,#26748,
#26749,#26750,#26751,#26752,#26753,#26754,#26755,#26756,#26757,#26758,#26759,
#26760,#26761,#26762,#26763,#26764,#26765,#26766,#26767,#26768,#26769,#26770,
#26771,#26772,#26773,#26774,#26775,#26776,#26777,#26778,#26779,#26780,#26781,
#26782,#26783,#26784,#26785,#26786,#26787,#26788,#26789,#26790,#26791,#26792,
#26793,#26794,#26795,#26796,#26797,#26798,#26799,#26800,#26801,#26802,#26803,
#26804,#26805,#26806,#26807,#26808,#26809,#26810,#26811,#26812,#26813,#26814,
#26815,#26816,#26817,#26818,#26819,#26820,#26821,#26822,#26823)),
 .UNSPECIFIED.,.T.,.F.,.F.,(4,1,1,1,2,1,1,1,4),(4,1,1,1,1,1,1,1,1,1,1,1,
1,1,1,1,1,1,1,1,1,1,1,1,1,1,1,1,1,1,1,1,1,1,1,1,1,1,1,1,1,1,1,1,1,1,1,1,
1,1,1,1,1,1,1,1,1,1,1,1,1,1,1,1,1,1,1,1,1,1,1,1,1,1,1,1,4),(-6.28318530717958,
-5.83438635666675,-4.9367884556411,-4.03919055461544,-3.14159265358979,
-2.24399475256414,-1.34639685153848,-0.448798950512828,0.),(0.,0.496040945303652,
0.992081890607303,1.48812283591095,1.98416378121461,2.48020472651826,2.97624567182191,
3.47228661712556,3.96832756242921,4.46436850773286,4.96040945303652,5.45645039834017,
5.95249134364382,6.44853228894747,6.94457323425112,7.44061417955477,7.93665512485842,
8.43269607016208,8.92873701546573,9.42477796076938,9.92081890607303,10.4168598513767,
10.9129007966803,11.408941741984,11.9049826872876,12.4010236325913,12.8970645778949,
13.3931055231986,13.8891464685022,14.3851874138059,14.8812283591095,15.3772693044132,
15.8733102497168,16.3693511950205,16.8653921403242,17.3614330856278,17.8574740309315,
18.3535149762351,18.8495559215388,19.3455968668424,19.8416378121461,20.3376787574497,
20.8337197027534,21.329760648057,21.8258015933607,22.3218425386643,22.817883483968,
23.3139244292716,23.8099653745753,24.3060063198789,24.8020472651826,25.2980882104862,
25.7941291557899,26.2901701010935,26.7862110463972,27.2822519917008,27.7782929370045,
28.2743338823081,28.7703748276118,29.2664157729154,29.7624567182191,30.2584976635227,
30.7545386088264,31.25057955413,31.7466204994337,32.2426614447374,32.738702390041,
33.2347433353447,33.7307842806483,34.226825225952,34.7228661712556,35.2189071165593,
35.7149480618629,36.2109890071666,36.7070299524702,37.2030708977739,37.6991118430775),
 .UNSPECIFIED.);
#97=B_SPLINE_SURFACE_WITH_KNOTS('',3,3,((#27026,#27027,#27028,#27029,#27030,
#27031,#27032,#27033,#27034,#27035,#27036,#27037,#27038,#27039,#27040,#27041,
#27042,#27043,#27044,#27045,#27046,#27047,#27048,#27049,#27050,#27051,#27052,
#27053,#27054,#27055,#27056,#27057,#27058,#27059,#27060,#27061,#27062,#27063,
#27064,#27065,#27066,#27067,#27068,#27069,#27070,#27071,#27072,#27073,#27074,
#27075,#27076,#27077,#27078,#27079,#27080,#27081,#27082,#27083,#27084,#27085,
#27086,#27087,#27088,#27089,#27090,#27091,#27092,#27093,#27094,#27095,#27096,
#27097,#27098,#27099,#27100,#27101,#27102,#27103,#27104),(#27105,#27106,
#27107,#27108,#27109,#27110,#27111,#27112,#27113,#27114,#27115,#27116,#27117,
#27118,#27119,#27120,#27121,#27122,#27123,#27124,#27125,#27126,#27127,#27128,
#27129,#27130,#27131,#27132,#27133,#27134,#27135,#27136,#27137,#27138,#27139,
#27140,#27141,#27142,#27143,#27144,#27145,#27146,#27147,#27148,#27149,#27150,
#27151,#27152,#27153,#27154,#27155,#27156,#27157,#27158,#27159,#27160,#27161,
#27162,#27163,#27164,#27165,#27166,#27167,#27168,#27169,#27170,#27171,#27172,
#27173,#27174,#27175,#27176,#27177,#27178,#27179,#27180,#27181,#27182,#27183),
(#27184,#27185,#27186,#27187,#27188,#27189,#27190,#27191,#27192,#27193,
#27194,#27195,#27196,#27197,#27198,#27199,#27200,#27201,#27202,#27203,#27204,
#27205,#27206,#27207,#27208,#27209,#27210,#27211,#27212,#27213,#27214,#27215,
#27216,#27217,#27218,#27219,#27220,#27221,#27222,#27223,#27224,#27225,#27226,
#27227,#27228,#27229,#27230,#27231,#27232,#27233,#27234,#27235,#27236,#27237,
#27238,#27239,#27240,#27241,#27242,#27243,#27244,#27245,#27246,#27247,#27248,
#27249,#27250,#27251,#27252,#27253,#27254,#27255,#27256,#27257,#27258,#27259,
#27260,#27261,#27262),(#27263,#27264,#27265,#27266,#27267,#27268,#27269,
#27270,#27271,#27272,#27273,#27274,#27275,#27276,#27277,#27278,#27279,#27280,
#27281,#27282,#27283,#27284,#27285,#27286,#27287,#27288,#27289,#27290,#27291,
#27292,#27293,#27294,#27295,#27296,#27297,#27298,#27299,#27300,#27301,#27302,
#27303,#27304,#27305,#27306,#27307,#27308,#27309,#27310,#27311,#27312,#27313,
#27314,#27315,#27316,#27317,#27318,#27319,#27320,#27321,#27322,#27323,#27324,
#27325,#27326,#27327,#27328,#27329,#27330,#27331,#27332,#27333,#27334,#27335,
#27336,#27337,#27338,#27339,#27340,#27341),(#27342,#27343,#27344,#27345,
#27346,#27347,#27348,#27349,#27350,#27351,#27352,#27353,#27354,#27355,#27356,
#27357,#27358,#27359,#27360,#27361,#27362,#27363,#27364,#27365,#27366,#27367,
#27368,#27369,#27370,#27371,#27372,#27373,#27374,#27375,#27376,#27377,#27378,
#27379,#27380,#27381,#27382,#27383,#27384,#27385,#27386,#27387,#27388,#27389,
#27390,#27391,#27392,#27393,#27394,#27395,#27396,#27397,#27398,#27399,#27400,
#27401,#27402,#27403,#27404,#27405,#27406,#27407,#27408,#27409,#27410,#27411,
#27412,#27413,#27414,#27415,#27416,#27417,#27418,#27419,#27420),(#27421,
#27422,#27423,#27424,#27425,#27426,#27427,#27428,#27429,#27430,#27431,#27432,
#27433,#27434,#27435,#27436,#27437,#27438,#27439,#27440,#27441,#27442,#27443,
#27444,#27445,#27446,#27447,#27448,#27449,#27450,#27451,#27452,#27453,#27454,
#27455,#27456,#27457,#27458,#27459,#27460,#27461,#27462,#27463,#27464,#27465,
#27466,#27467,#27468,#27469,#27470,#27471,#27472,#27473,#27474,#27475,#27476,
#27477,#27478,#27479,#27480,#27481,#27482,#27483,#27484,#27485,#27486,#27487,
#27488,#27489,#27490,#27491,#27492,#27493,#27494,#27495,#27496,#27497,#27498,
#27499),(#27500,#27501,#27502,#27503,#27504,#27505,#27506,#27507,#27508,
#27509,#27510,#27511,#27512,#27513,#27514,#27515,#27516,#27517,#27518,#27519,
#27520,#27521,#27522,#27523,#27524,#27525,#27526,#27527,#27528,#27529,#27530,
#27531,#27532,#27533,#27534,#27535,#27536,#27537,#27538,#27539,#27540,#27541,
#27542,#27543,#27544,#27545,#27546,#27547,#27548,#27549,#27550,#27551,#27552,
#27553,#27554,#27555,#27556,#27557,#27558,#27559,#27560,#27561,#27562,#27563,
#27564,#27565,#27566,#27567,#27568,#27569,#27570,#27571,#27572,#27573,#27574,
#27575,#27576,#27577,#27578),(#27579,#27580,#27581,#27582,#27583,#27584,
#27585,#27586,#27587,#27588,#27589,#27590,#27591,#27592,#27593,#27594,#27595,
#27596,#27597,#27598,#27599,#27600,#27601,#27602,#27603,#27604,#27605,#27606,
#27607,#27608,#27609,#27610,#27611,#27612,#27613,#27614,#27615,#27616,#27617,
#27618,#27619,#27620,#27621,#27622,#27623,#27624,#27625,#27626,#27627,#27628,
#27629,#27630,#27631,#27632,#27633,#27634,#27635,#27636,#27637,#27638,#27639,
#27640,#27641,#27642,#27643,#27644,#27645,#27646,#27647,#27648,#27649,#27650,
#27651,#27652,#27653,#27654,#27655,#27656,#27657),(#27658,#27659,#27660,
#27661,#27662,#27663,#27664,#27665,#27666,#27667,#27668,#27669,#27670,#27671,
#27672,#27673,#27674,#27675,#27676,#27677,#27678,#27679,#27680,#27681,#27682,
#27683,#27684,#27685,#27686,#27687,#27688,#27689,#27690,#27691,#27692,#27693,
#27694,#27695,#27696,#27697,#27698,#27699,#27700,#27701,#27702,#27703,#27704,
#27705,#27706,#27707,#27708,#27709,#27710,#27711,#27712,#27713,#27714,#27715,
#27716,#27717,#27718,#27719,#27720,#27721,#27722,#27723,#27724,#27725,#27726,
#27727,#27728,#27729,#27730,#27731,#27732,#27733,#27734,#27735,#27736),
(#27737,#27738,#27739,#27740,#27741,#27742,#27743,#27744,#27745,#27746,
#27747,#27748,#27749,#27750,#27751,#27752,#27753,#27754,#27755,#27756,#27757,
#27758,#27759,#27760,#27761,#27762,#27763,#27764,#27765,#27766,#27767,#27768,
#27769,#27770,#27771,#27772,#27773,#27774,#27775,#27776,#27777,#27778,#27779,
#27780,#27781,#27782,#27783,#27784,#27785,#27786,#27787,#27788,#27789,#27790,
#27791,#27792,#27793,#27794,#27795,#27796,#27797,#27798,#27799,#27800,#27801,
#27802,#27803,#27804,#27805,#27806,#27807,#27808,#27809,#27810,#27811,#27812,
#27813,#27814,#27815),(#27816,#27817,#27818,#27819,#27820,#27821,#27822,
#27823,#27824,#27825,#27826,#27827,#27828,#27829,#27830,#27831,#27832,#27833,
#27834,#27835,#27836,#27837,#27838,#27839,#27840,#27841,#27842,#27843,#27844,
#27845,#27846,#27847,#27848,#27849,#27850,#27851,#27852,#27853,#27854,#27855,
#27856,#27857,#27858,#27859,#27860,#27861,#27862,#27863,#27864,#27865,#27866,
#27867,#27868,#27869,#27870,#27871,#27872,#27873,#27874,#27875,#27876,#27877,
#27878,#27879,#27880,#27881,#27882,#27883,#27884,#27885,#27886,#27887,#27888,
#27889,#27890,#27891,#27892,#27893,#27894),(#27895,#27896,#27897,#27898,
#27899,#27900,#27901,#27902,#27903,#27904,#27905,#27906,#27907,#27908,#27909,
#27910,#27911,#27912,#27913,#27914,#27915,#27916,#27917,#27918,#27919,#27920,
#27921,#27922,#27923,#27924,#27925,#27926,#27927,#27928,#27929,#27930,#27931,
#27932,#27933,#27934,#27935,#27936,#27937,#27938,#27939,#27940,#27941,#27942,
#27943,#27944,#27945,#27946,#27947,#27948,#27949,#27950,#27951,#27952,#27953,
#27954,#27955,#27956,#27957,#27958,#27959,#27960,#27961,#27962,#27963,#27964,
#27965,#27966,#27967,#27968,#27969,#27970,#27971,#27972,#27973)),
 .UNSPECIFIED.,.T.,.F.,.F.,(4,1,1,1,2,1,1,1,4),(4,1,1,1,1,1,1,1,1,1,1,1,
1,1,1,1,1,1,1,1,1,1,1,1,1,1,1,1,1,1,1,1,1,1,1,1,1,1,1,1,1,1,1,1,1,1,1,1,
1,1,1,1,1,1,1,1,1,1,1,1,1,1,1,1,1,1,1,1,1,1,1,1,1,1,1,1,4),(6.28318530717958,
6.73198425769241,7.62958215871806,8.52718005974372,9.42477796076937,10.322375861795,
11.2199737628207,12.1175716638463,12.5663706143592),(0.,0.496040945303652,
0.992081890607303,1.48812283591095,1.98416378121461,2.48020472651826,2.97624567182191,
3.47228661712556,3.96832756242921,4.46436850773286,4.96040945303652,5.45645039834017,
5.95249134364382,6.44853228894747,6.94457323425112,7.44061417955477,7.93665512485842,
8.43269607016208,8.92873701546573,9.42477796076938,9.92081890607303,10.4168598513767,
10.9129007966803,11.408941741984,11.9049826872876,12.4010236325913,12.8970645778949,
13.3931055231986,13.8891464685022,14.3851874138059,14.8812283591095,15.3772693044132,
15.8733102497168,16.3693511950205,16.8653921403242,17.3614330856278,17.8574740309315,
18.3535149762351,18.8495559215388,19.3455968668424,19.8416378121461,20.3376787574497,
20.8337197027534,21.329760648057,21.8258015933607,22.3218425386643,22.817883483968,
23.3139244292716,23.8099653745753,24.3060063198789,24.8020472651826,25.2980882104862,
25.7941291557899,26.2901701010935,26.7862110463972,27.2822519917008,27.7782929370045,
28.2743338823081,28.7703748276118,29.2664157729154,29.7624567182191,30.2584976635227,
30.7545386088264,31.25057955413,31.7466204994337,32.2426614447374,32.738702390041,
33.2347433353447,33.7307842806483,34.226825225952,34.7228661712556,35.2189071165593,
35.7149480618629,36.2109890071666,36.7070299524702,37.2030708977739,37.6991118430775),
 .UNSPECIFIED.);
#98=TOROIDAL_SURFACE('',#3875,6.10845002480549,0.3);
#99=TOROIDAL_SURFACE('',#3881,6.107959450045,0.3);
#100=TOROIDAL_SURFACE('',#3887,4.18902817623056,0.3);
#101=TOROIDAL_SURFACE('',#3894,6.1096023907077,0.3);
#102=TOROIDAL_SURFACE('',#3901,6.10941276264524,0.3);
#103=TOROIDAL_SURFACE('',#3906,6.1087216021292,0.3);
#104=TOROIDAL_SURFACE('',#3914,6.1086273903848,0.3);
#105=TOROIDAL_SURFACE('',#3916,6.10778208446569,0.3);
#106=TOROIDAL_SURFACE('',#3921,6.10767319978801,0.3);
#107=TOROIDAL_SURFACE('',#3926,6.1069775362949,0.3);
#108=TOROIDAL_SURFACE('',#3934,6.10683442041659,0.3);
#109=TOROIDAL_SURFACE('',#3939,4.12329516333974,0.3);
#110=TOROIDAL_SURFACE('',#3991,6.10923539706593,0.3);
#111=TOROIDAL_SURFACE('',#3998,6.1088989677085,0.3);
#112=TOROIDAL_SURFACE('',#4003,6.1074958342087,0.3);
#113=TOROIDAL_SURFACE('',#4010,6.1071549018742,0.3);
#114=TOROIDAL_SURFACE('',#4065,4.58180150972878,0.3);
#115=TOROIDAL_SURFACE('',#4067,4.58180150972878,0.3);
#116=SHAPE_REPRESENTATION_RELATIONSHIP('SRR','None',#28093,#126);
#117=SHAPE_REPRESENTATION_RELATIONSHIP('SRR','None',#28094,#127);
#118=SHAPE_REPRESENTATION_RELATIONSHIP('SRR','None',#28095,#128);
#119=SHAPE_REPRESENTATION_RELATIONSHIP('SRR','None',#28096,#129);
#120=SHAPE_REPRESENTATION_RELATIONSHIP('SRR','None',#28097,#130);
#121=SHAPE_REPRESENTATION_RELATIONSHIP('SRR','None',#28098,#131);
#122=SHAPE_REPRESENTATION_RELATIONSHIP('SRR','None',#28099,#132);
#123=SHAPE_REPRESENTATION_RELATIONSHIP('SRR','None',#28100,#133);
#124=SHAPE_REPRESENTATION_RELATIONSHIP('SRR','None',#28101,#134);
#125=SHAPE_REPRESENTATION_RELATIONSHIP('SRR','None',#28102,#135);
#126=ADVANCED_BREP_SHAPE_REPRESENTATION('',(#146),#28045);
#127=ADVANCED_BREP_SHAPE_REPRESENTATION('',(#147),#28046);
#128=ADVANCED_BREP_SHAPE_REPRESENTATION('',(#148),#28047);
#129=ADVANCED_BREP_SHAPE_REPRESENTATION('',(#149),#28048);
#130=ADVANCED_BREP_SHAPE_REPRESENTATION('',(#150),#28049);
#131=ADVANCED_BREP_SHAPE_REPRESENTATION('',(#151),#28050);
#132=ADVANCED_BREP_SHAPE_REPRESENTATION('',(#152),#28051);
#133=ADVANCED_BREP_SHAPE_REPRESENTATION('',(#53),#28052);
#134=ADVANCED_BREP_SHAPE_REPRESENTATION('',(#153),#28053);
#135=ADVANCED_BREP_SHAPE_REPRESENTATION('',(#154),#28054);
#136=STYLED_ITEM('',(#28152),#146);
#137=STYLED_ITEM('',(#28152),#147);
#138=STYLED_ITEM('',(#28152),#148);
#139=STYLED_ITEM('',(#28152),#149);
#140=STYLED_ITEM('',(#28153),#150);
#141=STYLED_ITEM('',(#28153),#151);
#142=STYLED_ITEM('',(#28152),#152);
#143=STYLED_ITEM('',(#28152),#53);
#144=STYLED_ITEM('',(#28152),#153);
#145=STYLED_ITEM('',(#28152),#154);
#146=MANIFOLD_SOLID_BREP('Body1',#3677);
#147=MANIFOLD_SOLID_BREP('Body1',#3678);
#148=MANIFOLD_SOLID_BREP('Body1',#3679);
#149=MANIFOLD_SOLID_BREP('Body1',#3680);
#150=MANIFOLD_SOLID_BREP('Body1',#3681);
#151=MANIFOLD_SOLID_BREP('Body1',#3682);
#152=MANIFOLD_SOLID_BREP('Body1',#3683);
#153=MANIFOLD_SOLID_BREP('Body1',#3687);
#154=MANIFOLD_SOLID_BREP('Body1',#3688);
#155=CONICAL_SURFACE('',#3808,7.20746054905241,0.610790367386849);
#156=CONICAL_SURFACE('',#3813,7.36529369971832,0.557210682142491);
#157=CONICAL_SURFACE('',#3815,7.36790580323689,0.610790367386849);
#158=CONICAL_SURFACE('',#3819,6.97561584944256,0.658634244892553);
#159=CONICAL_SURFACE('',#3821,6.41628586403442,0.000295609290232646);
#160=CONICAL_SURFACE('',#3825,6.40906719549494,0.00029560929023293);
#161=CONICAL_SURFACE('',#3833,6.40820475053297,0.000295609290233083);
#162=CONICAL_SURFACE('',#3837,6.40732538114918,0.000295609290232334);
#163=CONICAL_SURFACE('',#3841,6.40667124022599,0.000295609290231853);
#164=CONICAL_SURFACE('',#3879,6.40820475053297,0.000295609290233083);
#165=CONICAL_SURFACE('',#3898,6.40950758978419,0.000295609290232241);
#166=CONICAL_SURFACE('',#3910,6.40867450936473,0.000295609290232273);
#167=CONICAL_SURFACE('',#3919,6.40772765523458,0.000295609290232245);
#168=CONICAL_SURFACE('',#3930,6.40690599146347,0.000295609290233429);
#169=CONICAL_SURFACE('',#3995,6.40906719549494,0.00029560929023293);
#170=CONICAL_SURFACE('',#4007,6.40732538114918,0.000295609290232334);
#171=CONICAL_SURFACE('',#4077,6.97561584944256,0.682200217168611);
#172=CONICAL_SURFACE('',#4083,6.97638033209901,0.810344007057193);
#173=FACE_BOUND('',#588,.T.);
#174=FACE_BOUND('',#591,.T.);
#175=FACE_BOUND('',#600,.T.);
#176=FACE_BOUND('',#603,.T.);
#177=FACE_BOUND('',#610,.T.);
#178=FACE_BOUND('',#613,.T.);
#179=FACE_BOUND('',#615,.T.);
#180=FACE_BOUND('',#617,.T.);
#181=FACE_BOUND('',#632,.T.);
#182=FACE_BOUND('',#635,.T.);
#183=FACE_BOUND('',#640,.T.);
#184=FACE_BOUND('',#648,.T.);
#185=FACE_BOUND('',#652,.T.);
#186=FACE_BOUND('',#655,.T.);
#187=FACE_BOUND('',#659,.T.);
#188=FACE_BOUND('',#665,.T.);
#189=FACE_BOUND('',#669,.T.);
#190=FACE_BOUND('',#672,.T.);
#191=FACE_BOUND('',#689,.T.);
#192=FACE_BOUND('',#691,.T.);
#193=FACE_BOUND('',#709,.T.);
#194=FACE_BOUND('',#711,.T.);
#195=FACE_BOUND('',#713,.T.);
#196=FACE_BOUND('',#785,.T.);
#197=FACE_BOUND('',#789,.T.);
#198=FACE_BOUND('',#793,.T.);
#199=FACE_BOUND('',#798,.T.);
#200=FACE_BOUND('',#802,.T.);
#201=FACE_BOUND('',#814,.T.);
#202=FACE_BOUND('',#816,.T.);
#203=PLANE('',#3806);
#204=PLANE('',#3827);
#205=PLANE('',#3831);
#206=PLANE('',#3843);
#207=PLANE('',#3847);
#208=PLANE('',#3850);
#209=PLANE('',#3872);
#210=PLANE('',#3883);
#211=PLANE('',#3885);
#212=PLANE('',#3886);
#213=PLANE('',#3893);
#214=PLANE('',#3900);
#215=PLANE('',#3904);
#216=PLANE('',#3912);
#217=PLANE('',#3924);
#218=PLANE('',#3932);
#219=PLANE('',#3937);
#220=PLANE('',#3943);
#221=PLANE('',#3954);
#222=PLANE('',#3955);
#223=PLANE('',#3956);
#224=PLANE('',#3957);
#225=PLANE('',#3958);
#226=PLANE('',#3959);
#227=PLANE('',#3960);
#228=PLANE('',#3961);
#229=PLANE('',#3978);
#230=PLANE('',#3987);
#231=PLANE('',#3988);
#232=PLANE('',#3989);
#233=PLANE('',#3997);
#234=PLANE('',#4001);
#235=PLANE('',#4009);
#236=PLANE('',#4013);
#237=PLANE('',#4015);
#238=PLANE('',#4016);
#239=PLANE('',#4035);
#240=PLANE('',#4057);
#241=PLANE('',#4058);
#242=PLANE('',#4063);
#243=PLANE('',#4071);
#244=PLANE('',#4080);
#245=PLANE('',#4085);
#246=PLANE('',#4093);
#247=PLANE('',#4094);
#248=PLANE('',#4095);
#249=PLANE('',#4096);
#250=PLANE('',#4097);
#251=PLANE('',#4098);
#252=PLANE('',#4099);
#253=PLANE('',#4100);
#254=PLANE('',#4102);
#255=PLANE('',#4103);
#256=CIRCLE('',#3804,5.);
#257=CIRCLE('',#3805,5.);
#258=CIRCLE('',#3807,3.44589712386029);
#259=CIRCLE('',#3809,7.52312685038423);
#260=CIRCLE('',#3810,6.89179424772059);
#261=CIRCLE('',#3812,7.52312685038423);
#262=CIRCLE('',#3814,7.20746054905241);
#263=CIRCLE('',#3816,7.52835105742136);
#264=CIRCLE('',#3818,7.52835105742136);
#265=CIRCLE('',#3820,6.42288064146375);
#266=CIRCLE('',#3822,6.40969108660508);
#267=CIRCLE('',#3824,6.40969108660508);
#268=CIRCLE('',#3826,6.40881029802658);
#269=CIRCLE('',#3828,6.41550316824698);
#270=CIRCLE('',#3830,6.41550316824698);
#271=CIRCLE('',#3832,6.40853872070288);
#272=CIRCLE('',#3834,6.40787078036307);
#273=CIRCLE('',#3836,6.40787078036307);
#274=CIRCLE('',#3838,6.40706623219228);
#275=CIRCLE('',#3840,6.40706623219228);
#276=CIRCLE('',#3842,6.4065967297173);
#277=CIRCLE('',#3844,4.66385643997278);
#278=CIRCLE('',#3846,4.66385643997278);
#279=CIRCLE('',#3848,3.44589712386029);
#280=CIRCLE('',#3853,1.77625);
#281=CIRCLE('',#3867,2.204);
#282=CIRCLE('',#3868,2.204);
#283=CIRCLE('',#3869,2.204);
#284=CIRCLE('',#3871,1.77625);
#285=CIRCLE('',#3873,6.107959450045);
#286=CIRCLE('',#3874,6.10778208446569);
#287=CIRCLE('',#3876,6.10845002480549);
#288=CIRCLE('',#3877,0.3);
#289=CIRCLE('',#3878,6.40845001169777);
#290=CIRCLE('',#3880,6.40795943693727);
#291=CIRCLE('',#3882,0.3);
#292=CIRCLE('',#3884,6.1086273903848);
#293=CIRCLE('',#3888,4.18902817623056);
#294=CIRCLE('',#3889,0.3);
#295=CIRCLE('',#3890,4.48902817623056);
#296=CIRCLE('',#3892,4.48902817623056);
#297=CIRCLE('',#3895,6.1096023907077);
#298=CIRCLE('',#3896,0.3);
#299=CIRCLE('',#3897,6.40960237759997);
#300=CIRCLE('',#3899,6.40941274953751);
#301=CIRCLE('',#3902,0.3);
#302=CIRCLE('',#3903,6.10941276264524);
#303=CIRCLE('',#3905,2.21164758166987);
#304=CIRCLE('',#3907,6.1087216021292);
#305=CIRCLE('',#3908,0.3);
#306=CIRCLE('',#3909,6.40872158902147);
#307=CIRCLE('',#3911,6.40862737727707);
#308=CIRCLE('',#3913,2.21164758166987);
#309=CIRCLE('',#3915,0.3);
#310=CIRCLE('',#3917,0.3);
#311=CIRCLE('',#3918,6.40778207135796);
#312=CIRCLE('',#3920,6.40767318668028);
#313=CIRCLE('',#3922,0.3);
#314=CIRCLE('',#3923,6.10767319978801);
#315=CIRCLE('',#3925,2.21164758166987);
#316=CIRCLE('',#3927,6.1069775362949);
#317=CIRCLE('',#3928,0.3);
#318=CIRCLE('',#3929,6.40697752318717);
#319=CIRCLE('',#3931,6.40683440730886);
#320=CIRCLE('',#3933,2.21164758166987);
#321=CIRCLE('',#3935,0.3);
#322=CIRCLE('',#3936,6.10683442041659);
#323=CIRCLE('',#3938,4.42329516333974);
#324=CIRCLE('',#3940,4.42329516333974);
#325=CIRCLE('',#3941,0.3);
#326=CIRCLE('',#3942,4.12329516333974);
#327=CIRCLE('',#3949,4.433);
#328=CIRCLE('',#3950,4.433);
#329=CIRCLE('',#3952,3.72275);
#330=CIRCLE('',#3953,3.72275);
#331=CIRCLE('',#3964,3.72275);
#332=CIRCLE('',#3971,4.433);
#333=CIRCLE('',#3972,4.433);
#334=CIRCLE('',#3974,3.72275);
#335=CIRCLE('',#3976,1.77625);
#336=CIRCLE('',#3977,1.77625);
#337=CIRCLE('',#3979,2.204);
#338=CIRCLE('',#3980,2.204);
#339=CIRCLE('',#3982,2.204);
#340=CIRCLE('',#3983,2.204);
#341=CIRCLE('',#3985,5.42440960677665);
#342=CIRCLE('',#3986,5.42440960677665);
#343=CIRCLE('',#3992,6.10923539706593);
#344=CIRCLE('',#3993,0.3);
#345=CIRCLE('',#3994,6.4092353839582);
#346=CIRCLE('',#3996,6.40889895460077);
#347=CIRCLE('',#3999,0.3);
#348=CIRCLE('',#4000,6.1088989677085);
#349=CIRCLE('',#4004,6.1074958342087);
#350=CIRCLE('',#4005,0.3);
#351=CIRCLE('',#4006,6.40749582110097);
#352=CIRCLE('',#4008,6.40715488876647);
#353=CIRCLE('',#4011,0.3);
#354=CIRCLE('',#4012,6.1071549018742);
#355=CIRCLE('',#4018,3.22275);
#356=CIRCLE('',#4032,3.22275);
#357=CIRCLE('',#4036,3.933);
#358=CIRCLE('',#4039,3.933);
#359=CIRCLE('',#4055,5.);
#360=CIRCLE('',#4056,5.);
#361=CIRCLE('',#4061,4.88180150972878);
#362=CIRCLE('',#4062,4.88180150972878);
#363=CIRCLE('',#4064,4.58180150972878);
#364=CIRCLE('',#4066,0.3);
#365=CIRCLE('',#4068,4.58180150972878);
#366=CIRCLE('',#4069,0.3);
#367=CIRCLE('',#4070,4.88180150972878);
#368=CIRCLE('',#4072,4.88180150972878);
#369=CIRCLE('',#4075,2.204);
#370=CIRCLE('',#4076,2.204);
#371=CIRCLE('',#4078,7.52835105742136);
#372=CIRCLE('',#4079,6.42288064146375);
#373=CIRCLE('',#4082,7.52835105742136);
#374=CIRCLE('',#4084,6.42440960677665);
#375=CIRCLE('',#4088,4.433);
#376=CIRCLE('',#4089,4.433);
#377=CIRCLE('',#4091,3.72275);
#378=CIRCLE('',#4092,3.72275);
#379=FACE_OUTER_BOUND('',#585,.T.);
#380=FACE_OUTER_BOUND('',#586,.T.);
#381=FACE_OUTER_BOUND('',#587,.T.);
#382=FACE_OUTER_BOUND('',#589,.T.);
#383=FACE_OUTER_BOUND('',#590,.T.);
#384=FACE_OUTER_BOUND('',#592,.T.);
#385=FACE_OUTER_BOUND('',#593,.T.);
#386=FACE_OUTER_BOUND('',#594,.T.);
#387=FACE_OUTER_BOUND('',#595,.T.);
#388=FACE_OUTER_BOUND('',#596,.T.);
#389=FACE_OUTER_BOUND('',#597,.T.);
#390=FACE_OUTER_BOUND('',#598,.T.);
#391=FACE_OUTER_BOUND('',#599,.T.);
#392=FACE_OUTER_BOUND('',#601,.T.);
#393=FACE_OUTER_BOUND('',#602,.T.);
#394=FACE_OUTER_BOUND('',#604,.T.);
#395=FACE_OUTER_BOUND('',#605,.T.);
#396=FACE_OUTER_BOUND('',#606,.T.);
#397=FACE_OUTER_BOUND('',#607,.T.);
#398=FACE_OUTER_BOUND('',#608,.T.);
#399=FACE_OUTER_BOUND('',#609,.T.);
#400=FACE_OUTER_BOUND('',#611,.T.);
#401=FACE_OUTER_BOUND('',#612,.T.);
#402=FACE_OUTER_BOUND('',#614,.T.);
#403=FACE_OUTER_BOUND('',#616,.T.);
#404=FACE_OUTER_BOUND('',#618,.T.);
#405=FACE_OUTER_BOUND('',#619,.T.);
#406=FACE_OUTER_BOUND('',#620,.T.);
#407=FACE_OUTER_BOUND('',#621,.T.);
#408=FACE_OUTER_BOUND('',#622,.T.);
#409=FACE_OUTER_BOUND('',#623,.T.);
#410=FACE_OUTER_BOUND('',#624,.T.);
#411=FACE_OUTER_BOUND('',#625,.T.);
#412=FACE_OUTER_BOUND('',#626,.T.);
#413=FACE_OUTER_BOUND('',#627,.T.);
#414=FACE_OUTER_BOUND('',#628,.T.);
#415=FACE_OUTER_BOUND('',#629,.T.);
#416=FACE_OUTER_BOUND('',#630,.T.);
#417=FACE_OUTER_BOUND('',#631,.T.);
#418=FACE_OUTER_BOUND('',#633,.T.);
#419=FACE_OUTER_BOUND('',#634,.T.);
#420=FACE_OUTER_BOUND('',#636,.T.);
#421=FACE_OUTER_BOUND('',#637,.T.);
#422=FACE_OUTER_BOUND('',#638,.T.);
#423=FACE_OUTER_BOUND('',#639,.T.);
#424=FACE_OUTER_BOUND('',#641,.T.);
#425=FACE_OUTER_BOUND('',#642,.T.);
#426=FACE_OUTER_BOUND('',#643,.T.);
#427=FACE_OUTER_BOUND('',#644,.T.);
#428=FACE_OUTER_BOUND('',#645,.T.);
#429=FACE_OUTER_BOUND('',#646,.T.);
#430=FACE_OUTER_BOUND('',#647,.T.);
#431=FACE_OUTER_BOUND('',#649,.T.);
#432=FACE_OUTER_BOUND('',#650,.T.);
#433=FACE_OUTER_BOUND('',#651,.T.);
#434=FACE_OUTER_BOUND('',#653,.T.);
#435=FACE_OUTER_BOUND('',#654,.T.);
#436=FACE_OUTER_BOUND('',#656,.T.);
#437=FACE_OUTER_BOUND('',#657,.T.);
#438=FACE_OUTER_BOUND('',#658,.T.);
#439=FACE_OUTER_BOUND('',#660,.T.);
#440=FACE_OUTER_BOUND('',#661,.T.);
#441=FACE_OUTER_BOUND('',#662,.T.);
#442=FACE_OUTER_BOUND('',#663,.T.);
#443=FACE_OUTER_BOUND('',#664,.T.);
#444=FACE_OUTER_BOUND('',#666,.T.);
#445=FACE_OUTER_BOUND('',#667,.T.);
#446=FACE_OUTER_BOUND('',#668,.T.);
#447=FACE_OUTER_BOUND('',#670,.T.);
#448=FACE_OUTER_BOUND('',#671,.T.);
#449=FACE_OUTER_BOUND('',#673,.T.);
#450=FACE_OUTER_BOUND('',#674,.T.);
#451=FACE_OUTER_BOUND('',#675,.T.);
#452=FACE_OUTER_BOUND('',#676,.T.);
#453=FACE_OUTER_BOUND('',#677,.T.);
#454=FACE_OUTER_BOUND('',#678,.T.);
#455=FACE_OUTER_BOUND('',#679,.T.);
#456=FACE_OUTER_BOUND('',#680,.T.);
#457=FACE_OUTER_BOUND('',#681,.T.);
#458=FACE_OUTER_BOUND('',#682,.T.);
#459=FACE_OUTER_BOUND('',#683,.T.);
#460=FACE_OUTER_BOUND('',#684,.T.);
#461=FACE_OUTER_BOUND('',#685,.T.);
#462=FACE_OUTER_BOUND('',#686,.T.);
#463=FACE_OUTER_BOUND('',#687,.T.);
#464=FACE_OUTER_BOUND('',#688,.T.);
#465=FACE_OUTER_BOUND('',#690,.T.);
#466=FACE_OUTER_BOUND('',#692,.T.);
#467=FACE_OUTER_BOUND('',#693,.T.);
#468=FACE_OUTER_BOUND('',#694,.T.);
#469=FACE_OUTER_BOUND('',#695,.T.);
#470=FACE_OUTER_BOUND('',#696,.T.);
#471=FACE_OUTER_BOUND('',#697,.T.);
#472=FACE_OUTER_BOUND('',#698,.T.);
#473=FACE_OUTER_BOUND('',#699,.T.);
#474=FACE_OUTER_BOUND('',#700,.T.);
#475=FACE_OUTER_BOUND('',#701,.T.);
#476=FACE_OUTER_BOUND('',#702,.T.);
#477=FACE_OUTER_BOUND('',#703,.T.);
#478=FACE_OUTER_BOUND('',#704,.T.);
#479=FACE_OUTER_BOUND('',#705,.T.);
#480=FACE_OUTER_BOUND('',#706,.T.);
#481=FACE_OUTER_BOUND('',#707,.T.);
#482=FACE_OUTER_BOUND('',#708,.T.);
#483=FACE_OUTER_BOUND('',#710,.T.);
#484=FACE_OUTER_BOUND('',#712,.T.);
#485=FACE_OUTER_BOUND('',#714,.T.);
#486=FACE_OUTER_BOUND('',#715,.T.);
#487=FACE_OUTER_BOUND('',#716,.T.);
#488=FACE_OUTER_BOUND('',#717,.T.);
#489=FACE_OUTER_BOUND('',#718,.T.);
#490=FACE_OUTER_BOUND('',#719,.T.);
#491=FACE_OUTER_BOUND('',#720,.T.);
#492=FACE_OUTER_BOUND('',#721,.T.);
#493=FACE_OUTER_BOUND('',#722,.T.);
#494=FACE_OUTER_BOUND('',#723,.T.);
#495=FACE_OUTER_BOUND('',#724,.T.);
#496=FACE_OUTER_BOUND('',#725,.T.);
#497=FACE_OUTER_BOUND('',#726,.T.);
#498=FACE_OUTER_BOUND('',#727,.T.);
#499=FACE_OUTER_BOUND('',#728,.T.);
#500=FACE_OUTER_BOUND('',#729,.T.);
#501=FACE_OUTER_BOUND('',#730,.T.);
#502=FACE_OUTER_BOUND('',#731,.T.);
#503=FACE_OUTER_BOUND('',#732,.T.);
#504=FACE_OUTER_BOUND('',#733,.T.);
#505=FACE_OUTER_BOUND('',#734,.T.);
#506=FACE_OUTER_BOUND('',#735,.T.);
#507=FACE_OUTER_BOUND('',#736,.T.);
#508=FACE_OUTER_BOUND('',#737,.T.);
#509=FACE_OUTER_BOUND('',#738,.T.);
#510=FACE_OUTER_BOUND('',#739,.T.);
#511=FACE_OUTER_BOUND('',#740,.T.);
#512=FACE_OUTER_BOUND('',#741,.T.);
#513=FACE_OUTER_BOUND('',#742,.T.);
#514=FACE_OUTER_BOUND('',#743,.T.);
#515=FACE_OUTER_BOUND('',#744,.T.);
#516=FACE_OUTER_BOUND('',#745,.T.);
#517=FACE_OUTER_BOUND('',#746,.T.);
#518=FACE_OUTER_BOUND('',#747,.T.);
#519=FACE_OUTER_BOUND('',#748,.T.);
#520=FACE_OUTER_BOUND('',#749,.T.);
#521=FACE_OUTER_BOUND('',#750,.T.);
#522=FACE_OUTER_BOUND('',#751,.T.);
#523=FACE_OUTER_BOUND('',#752,.T.);
#524=FACE_OUTER_BOUND('',#753,.T.);
#525=FACE_OUTER_BOUND('',#754,.T.);
#526=FACE_OUTER_BOUND('',#755,.T.);
#527=FACE_OUTER_BOUND('',#756,.T.);
#528=FACE_OUTER_BOUND('',#757,.T.);
#529=FACE_OUTER_BOUND('',#758,.T.);
#530=FACE_OUTER_BOUND('',#759,.T.);
#531=FACE_OUTER_BOUND('',#760,.T.);
#532=FACE_OUTER_BOUND('',#761,.T.);
#533=FACE_OUTER_BOUND('',#762,.T.);
#534=FACE_OUTER_BOUND('',#763,.T.);
#535=FACE_OUTER_BOUND('',#764,.T.);
#536=FACE_OUTER_BOUND('',#765,.T.);
#537=FACE_OUTER_BOUND('',#766,.T.);
#538=FACE_OUTER_BOUND('',#767,.T.);
#539=FACE_OUTER_BOUND('',#768,.T.);
#540=FACE_OUTER_BOUND('',#769,.T.);
#541=FACE_OUTER_BOUND('',#770,.T.);
#542=FACE_OUTER_BOUND('',#771,.T.);
#543=FACE_OUTER_BOUND('',#772,.T.);
#544=FACE_OUTER_BOUND('',#773,.T.);
#545=FACE_OUTER_BOUND('',#774,.T.);
#546=FACE_OUTER_BOUND('',#775,.T.);
#547=FACE_OUTER_BOUND('',#776,.T.);
#548=FACE_OUTER_BOUND('',#777,.T.);
#549=FACE_OUTER_BOUND('',#778,.T.);
#550=FACE_OUTER_BOUND('',#779,.T.);
#551=FACE_OUTER_BOUND('',#780,.T.);
#552=FACE_OUTER_BOUND('',#781,.T.);
#553=FACE_OUTER_BOUND('',#782,.T.);
#554=FACE_OUTER_BOUND('',#783,.T.);
#555=FACE_OUTER_BOUND('',#784,.T.);
#556=FACE_OUTER_BOUND('',#786,.T.);
#557=FACE_OUTER_BOUND('',#787,.T.);
#558=FACE_OUTER_BOUND('',#788,.T.);
#559=FACE_OUTER_BOUND('',#790,.T.);
#560=FACE_OUTER_BOUND('',#791,.T.);
#561=FACE_OUTER_BOUND('',#792,.T.);
#562=FACE_OUTER_BOUND('',#794,.T.);
#563=FACE_OUTER_BOUND('',#795,.T.);
#564=FACE_OUTER_BOUND('',#796,.T.);
#565=FACE_OUTER_BOUND('',#797,.T.);
#566=FACE_OUTER_BOUND('',#799,.T.);
#567=FACE_OUTER_BOUND('',#800,.T.);
#568=FACE_OUTER_BOUND('',#801,.T.);
#569=FACE_OUTER_BOUND('',#803,.T.);
#570=FACE_OUTER_BOUND('',#804,.T.);
#571=FACE_OUTER_BOUND('',#805,.T.);
#572=FACE_OUTER_BOUND('',#806,.T.);
#573=FACE_OUTER_BOUND('',#807,.T.);
#574=FACE_OUTER_BOUND('',#808,.T.);
#575=FACE_OUTER_BOUND('',#809,.T.);
#576=FACE_OUTER_BOUND('',#810,.T.);
#577=FACE_OUTER_BOUND('',#811,.T.);
#578=FACE_OUTER_BOUND('',#812,.T.);
#579=FACE_OUTER_BOUND('',#813,.T.);
#580=FACE_OUTER_BOUND('',#815,.T.);
#581=FACE_OUTER_BOUND('',#817,.T.);
#582=FACE_OUTER_BOUND('',#818,.T.);
#583=FACE_OUTER_BOUND('',#819,.T.);
#584=FACE_OUTER_BOUND('',#820,.T.);
#585=EDGE_LOOP('',(#2310,#2311,#2312,#2313,#2314,#2315));
#586=EDGE_LOOP('',(#2316,#2317,#2318,#2319));
#587=EDGE_LOOP('',(#2320));
#588=EDGE_LOOP('',(#2321));
#589=EDGE_LOOP('',(#2322,#2323,#2324,#2325));
#590=EDGE_LOOP('',(#2326,#2327,#2328,#2329));
#591=EDGE_LOOP('',(#2330,#2331));
#592=EDGE_LOOP('',(#2332,#2333,#2334,#2335));
#593=EDGE_LOOP('',(#2336,#2337,#2338,#2339));
#594=EDGE_LOOP('',(#2340,#2341,#2342,#2343));
#595=EDGE_LOOP('',(#2344,#2345,#2346,#2347));
#596=EDGE_LOOP('',(#2348,#2349,#2350,#2351));
#597=EDGE_LOOP('',(#2352,#2353,#2354,#2355));
#598=EDGE_LOOP('',(#2356,#2357,#2358,#2359));
#599=EDGE_LOOP('',(#2360));
#600=EDGE_LOOP('',(#2361));
#601=EDGE_LOOP('',(#2362,#2363,#2364,#2365));
#602=EDGE_LOOP('',(#2366));
#603=EDGE_LOOP('',(#2367));
#604=EDGE_LOOP('',(#2368,#2369,#2370,#2371));
#605=EDGE_LOOP('',(#2372,#2373,#2374,#2375));
#606=EDGE_LOOP('',(#2376,#2377,#2378,#2379));
#607=EDGE_LOOP('',(#2380,#2381,#2382,#2383));
#608=EDGE_LOOP('',(#2384,#2385,#2386,#2387));
#609=EDGE_LOOP('',(#2388));
#610=EDGE_LOOP('',(#2389));
#611=EDGE_LOOP('',(#2390,#2391,#2392,#2393));
#612=EDGE_LOOP('',(#2394));
#613=EDGE_LOOP('',(#2395));
#614=EDGE_LOOP('',(#2396,#2397,#2398,#2399));
#615=EDGE_LOOP('',(#2400,#2401));
#616=EDGE_LOOP('',(#2402));
#617=EDGE_LOOP('',(#2403));
#618=EDGE_LOOP('',(#2404,#2405,#2406,#2407,#2408));
#619=EDGE_LOOP('',(#2409,#2410,#2411,#2412,#2413));
#620=EDGE_LOOP('',(#2414,#2415,#2416,#2417,#2418,#2419));
#621=EDGE_LOOP('',(#2420,#2421,#2422,#2423,#2424,#2425));
#622=EDGE_LOOP('',(#2426,#2427,#2428,#2429,#2430));
#623=EDGE_LOOP('',(#2431,#2432,#2433,#2434,#2435));
#624=EDGE_LOOP('',(#2436,#2437,#2438,#2439,#2440));
#625=EDGE_LOOP('',(#2441,#2442,#2443,#2444,#2445));
#626=EDGE_LOOP('',(#2446,#2447,#2448,#2449,#2450));
#627=EDGE_LOOP('',(#2451,#2452,#2453,#2454,#2455));
#628=EDGE_LOOP('',(#2456,#2457,#2458,#2459,#2460));
#629=EDGE_LOOP('',(#2461,#2462,#2463,#2464,#2465));
#630=EDGE_LOOP('',(#2466,#2467,#2468,#2469,#2470,#2471));
#631=EDGE_LOOP('',(#2472));
#632=EDGE_LOOP('',(#2473,#2474,#2475,#2476,#2477,#2478,#2479,#2480,#2481,
#2482,#2483,#2484,#2485,#2486,#2487,#2488,#2489,#2490,#2491,#2492,#2493,
#2494,#2495,#2496,#2497,#2498,#2499,#2500,#2501,#2502,#2503));
#633=EDGE_LOOP('',(#2504,#2505,#2506,#2507,#2508,#2509));
#634=EDGE_LOOP('',(#2510));
#635=EDGE_LOOP('',(#2511));
#636=EDGE_LOOP('',(#2512,#2513,#2514,#2515));
#637=EDGE_LOOP('',(#2516,#2517,#2518,#2519));
#638=EDGE_LOOP('',(#2520,#2521,#2522,#2523));
#639=EDGE_LOOP('',(#2524));
#640=EDGE_LOOP('',(#2525));
#641=EDGE_LOOP('',(#2526,#2527,#2528,#2529,#2530,#2531,#2532,#2533,#2534,
#2535,#2536,#2537,#2538,#2539,#2540,#2541,#2542,#2543,#2544,#2545,#2546,
#2547,#2548,#2549,#2550,#2551,#2552,#2553,#2554,#2555,#2556,#2557,#2558,
#2559,#2560,#2561,#2562,#2563,#2564));
#642=EDGE_LOOP('',(#2565,#2566,#2567,#2568));
#643=EDGE_LOOP('',(#2569,#2570,#2571,#2572,#2573,#2574,#2575,#2576,#2577,
#2578,#2579,#2580,#2581,#2582,#2583,#2584,#2585,#2586,#2587,#2588,#2589,
#2590,#2591,#2592,#2593,#2594,#2595,#2596,#2597,#2598,#2599,#2600,#2601,
#2602,#2603,#2604,#2605,#2606,#2607,#2608));
#644=EDGE_LOOP('',(#2609,#2610,#2611,#2612));
#645=EDGE_LOOP('',(#2613,#2614,#2615,#2616));
#646=EDGE_LOOP('',(#2617,#2618,#2619,#2620));
#647=EDGE_LOOP('',(#2621));
#648=EDGE_LOOP('',(#2622));
#649=EDGE_LOOP('',(#2623,#2624,#2625,#2626));
#650=EDGE_LOOP('',(#2627,#2628,#2629,#2630));
#651=EDGE_LOOP('',(#2631));
#652=EDGE_LOOP('',(#2632));
#653=EDGE_LOOP('',(#2633,#2634,#2635,#2636));
#654=EDGE_LOOP('',(#2637));
#655=EDGE_LOOP('',(#2638));
#656=EDGE_LOOP('',(#2639,#2640,#2641,#2642));
#657=EDGE_LOOP('',(#2643,#2644,#2645,#2646));
#658=EDGE_LOOP('',(#2647));
#659=EDGE_LOOP('',(#2648));
#660=EDGE_LOOP('',(#2649,#2650,#2651,#2652));
#661=EDGE_LOOP('',(#2653,#2654,#2655,#2656));
#662=EDGE_LOOP('',(#2657,#2658,#2659,#2660));
#663=EDGE_LOOP('',(#2661,#2662,#2663,#2664));
#664=EDGE_LOOP('',(#2665));
#665=EDGE_LOOP('',(#2666));
#666=EDGE_LOOP('',(#2667,#2668,#2669,#2670));
#667=EDGE_LOOP('',(#2671,#2672,#2673,#2674));
#668=EDGE_LOOP('',(#2675));
#669=EDGE_LOOP('',(#2676));
#670=EDGE_LOOP('',(#2677,#2678,#2679,#2680));
#671=EDGE_LOOP('',(#2681));
#672=EDGE_LOOP('',(#2682));
#673=EDGE_LOOP('',(#2683,#2684,#2685,#2686));
#674=EDGE_LOOP('',(#2687));
#675=EDGE_LOOP('',(#2688,#2689,#2690,#2691));
#676=EDGE_LOOP('',(#2692,#2693,#2694,#2695));
#677=EDGE_LOOP('',(#2696,#2697,#2698,#2699));
#678=EDGE_LOOP('',(#2700,#2701,#2702,#2703));
#679=EDGE_LOOP('',(#2704,#2705,#2706,#2707));
#680=EDGE_LOOP('',(#2708,#2709,#2710,#2711));
#681=EDGE_LOOP('',(#2712,#2713,#2714,#2715));
#682=EDGE_LOOP('',(#2716,#2717,#2718,#2719));
#683=EDGE_LOOP('',(#2720,#2721,#2722,#2723));
#684=EDGE_LOOP('',(#2724,#2725,#2726,#2727));
#685=EDGE_LOOP('',(#2728,#2729,#2730,#2731));
#686=EDGE_LOOP('',(#2732,#2733,#2734,#2735));
#687=EDGE_LOOP('',(#2736,#2737,#2738,#2739));
#688=EDGE_LOOP('',(#2740,#2741,#2742,#2743,#2744,#2745));
#689=EDGE_LOOP('',(#2746,#2747,#2748,#2749));
#690=EDGE_LOOP('',(#2750,#2751,#2752,#2753,#2754,#2755));
#691=EDGE_LOOP('',(#2756,#2757,#2758,#2759));
#692=EDGE_LOOP('',(#2760,#2761,#2762,#2763));
#693=EDGE_LOOP('',(#2764,#2765,#2766,#2767,#2768,#2769));
#694=EDGE_LOOP('',(#2770,#2771,#2772,#2773,#2774));
#695=EDGE_LOOP('',(#2775,#2776,#2777,#2778,#2779));
#696=EDGE_LOOP('',(#2780,#2781,#2782,#2783,#2784));
#697=EDGE_LOOP('',(#2785,#2786,#2787,#2788,#2789));
#698=EDGE_LOOP('',(#2790,#2791,#2792,#2793,#2794,#2795,#2796,#2797,#2798,
#2799,#2800,#2801,#2802,#2803,#2804,#2805,#2806,#2807));
#699=EDGE_LOOP('',(#2808,#2809,#2810,#2811,#2812,#2813));
#700=EDGE_LOOP('',(#2814,#2815,#2816,#2817));
#701=EDGE_LOOP('',(#2818,#2819,#2820,#2821));
#702=EDGE_LOOP('',(#2822,#2823,#2824,#2825));
#703=EDGE_LOOP('',(#2826,#2827,#2828,#2829,#2830));
#704=EDGE_LOOP('',(#2831,#2832,#2833,#2834,#2835,#2836,#2837,#2838));
#705=EDGE_LOOP('',(#2839,#2840,#2841,#2842,#2843,#2844,#2845,#2846,#2847,
#2848,#2849,#2850,#2851,#2852,#2853,#2854,#2855,#2856,#2857,#2858,#2859));
#706=EDGE_LOOP('',(#2860,#2861,#2862,#2863,#2864,#2865,#2866,#2867,#2868,
#2869,#2870,#2871,#2872,#2873,#2874,#2875,#2876,#2877,#2878,#2879,#2880));
#707=EDGE_LOOP('',(#2881,#2882,#2883,#2884));
#708=EDGE_LOOP('',(#2885));
#709=EDGE_LOOP('',(#2886,#2887,#2888,#2889));
#710=EDGE_LOOP('',(#2890,#2891,#2892,#2893));
#711=EDGE_LOOP('',(#2894,#2895,#2896,#2897));
#712=EDGE_LOOP('',(#2898));
#713=EDGE_LOOP('',(#2899));
#714=EDGE_LOOP('',(#2900,#2901,#2902,#2903));
#715=EDGE_LOOP('',(#2904,#2905,#2906,#2907));
#716=EDGE_LOOP('',(#2908));
#717=EDGE_LOOP('',(#2909,#2910,#2911,#2912));
#718=EDGE_LOOP('',(#2913));
#719=EDGE_LOOP('',(#2914,#2915,#2916,#2917));
#720=EDGE_LOOP('',(#2918,#2919,#2920,#2921));
#721=EDGE_LOOP('',(#2922));
#722=EDGE_LOOP('',(#2923,#2924,#2925,#2926));
#723=EDGE_LOOP('',(#2927));
#724=EDGE_LOOP('',(#2928,#2929,#2930,#2931,#2932,#2933,#2934,#2935,#2936,
#2937,#2938,#2939,#2940,#2941,#2942,#2943,#2944,#2945,#2946,#2947,#2948,
#2949,#2950,#2951,#2952,#2953,#2954,#2955,#2956,#2957,#2958,#2959,#2960,
#2961,#2962,#2963,#2964,#2965,#2966,#2967,#2968,#2969,#2970,#2971,#2972,
#2973,#2974,#2975,#2976,#2977,#2978,#2979,#2980,#2981,#2982));
#725=EDGE_LOOP('',(#2983,#2984,#2985,#2986,#2987,#2988,#2989,#2990,#2991,
#2992,#2993,#2994,#2995,#2996,#2997,#2998,#2999,#3000,#3001,#3002,#3003,
#3004,#3005,#3006,#3007,#3008,#3009,#3010,#3011,#3012,#3013,#3014,#3015,
#3016,#3017,#3018,#3019,#3020,#3021,#3022,#3023,#3024,#3025,#3026,#3027,
#3028,#3029,#3030,#3031,#3032,#3033,#3034,#3035,#3036,#3037));
#726=EDGE_LOOP('',(#3038,#3039,#3040));
#727=EDGE_LOOP('',(#3041,#3042,#3043,#3044));
#728=EDGE_LOOP('',(#3045,#3046,#3047,#3048));
#729=EDGE_LOOP('',(#3049,#3050,#3051,#3052));
#730=EDGE_LOOP('',(#3053,#3054,#3055,#3056));
#731=EDGE_LOOP('',(#3057,#3058,#3059,#3060));
#732=EDGE_LOOP('',(#3061,#3062,#3063,#3064));
#733=EDGE_LOOP('',(#3065,#3066,#3067,#3068));
#734=EDGE_LOOP('',(#3069,#3070,#3071,#3072));
#735=EDGE_LOOP('',(#3073,#3074,#3075,#3076));
#736=EDGE_LOOP('',(#3077,#3078,#3079,#3080));
#737=EDGE_LOOP('',(#3081,#3082,#3083,#3084));
#738=EDGE_LOOP('',(#3085,#3086,#3087,#3088));
#739=EDGE_LOOP('',(#3089,#3090,#3091,#3092));
#740=EDGE_LOOP('',(#3093,#3094,#3095));
#741=EDGE_LOOP('',(#3096,#3097,#3098,#3099,#3100));
#742=EDGE_LOOP('',(#3101,#3102,#3103,#3104));
#743=EDGE_LOOP('',(#3105,#3106,#3107,#3108));
#744=EDGE_LOOP('',(#3109,#3110,#3111,#3112));
#745=EDGE_LOOP('',(#3113,#3114,#3115,#3116));
#746=EDGE_LOOP('',(#3117,#3118,#3119,#3120));
#747=EDGE_LOOP('',(#3121,#3122,#3123,#3124,#3125));
#748=EDGE_LOOP('',(#3126,#3127,#3128,#3129));
#749=EDGE_LOOP('',(#3130,#3131,#3132,#3133));
#750=EDGE_LOOP('',(#3134,#3135,#3136,#3137));
#751=EDGE_LOOP('',(#3138,#3139,#3140,#3141));
#752=EDGE_LOOP('',(#3142,#3143,#3144,#3145));
#753=EDGE_LOOP('',(#3146,#3147,#3148,#3149));
#754=EDGE_LOOP('',(#3150,#3151,#3152,#3153,#3154,#3155));
#755=EDGE_LOOP('',(#3156,#3157,#3158));
#756=EDGE_LOOP('',(#3159,#3160,#3161,#3162));
#757=EDGE_LOOP('',(#3163,#3164,#3165,#3166));
#758=EDGE_LOOP('',(#3167,#3168,#3169,#3170));
#759=EDGE_LOOP('',(#3171,#3172,#3173,#3174));
#760=EDGE_LOOP('',(#3175,#3176,#3177,#3178));
#761=EDGE_LOOP('',(#3179,#3180,#3181,#3182));
#762=EDGE_LOOP('',(#3183,#3184,#3185,#3186));
#763=EDGE_LOOP('',(#3187,#3188,#3189,#3190));
#764=EDGE_LOOP('',(#3191,#3192,#3193,#3194));
#765=EDGE_LOOP('',(#3195,#3196,#3197,#3198));
#766=EDGE_LOOP('',(#3199,#3200,#3201,#3202));
#767=EDGE_LOOP('',(#3203,#3204,#3205,#3206));
#768=EDGE_LOOP('',(#3207,#3208,#3209,#3210));
#769=EDGE_LOOP('',(#3211,#3212,#3213,#3214));
#770=EDGE_LOOP('',(#3215,#3216,#3217,#3218));
#771=EDGE_LOOP('',(#3219,#3220,#3221,#3222));
#772=EDGE_LOOP('',(#3223,#3224,#3225,#3226));
#773=EDGE_LOOP('',(#3227,#3228,#3229,#3230));
#774=EDGE_LOOP('',(#3231,#3232,#3233,#3234));
#775=EDGE_LOOP('',(#3235,#3236,#3237,#3238,#3239));
#776=EDGE_LOOP('',(#3240,#3241,#3242,#3243));
#777=EDGE_LOOP('',(#3244,#3245,#3246,#3247));
#778=EDGE_LOOP('',(#3248,#3249,#3250,#3251));
#779=EDGE_LOOP('',(#3252,#3253,#3254,#3255));
#780=EDGE_LOOP('',(#3256,#3257,#3258,#3259));
#781=EDGE_LOOP('',(#3260,#3261,#3262,#3263,#3264));
#782=EDGE_LOOP('',(#3265,#3266,#3267));
#783=EDGE_LOOP('',(#3268,#3269,#3270,#3271));
#784=EDGE_LOOP('',(#3272));
#785=EDGE_LOOP('',(#3273,#3274,#3275,#3276,#3277,#3278,#3279,#3280));
#786=EDGE_LOOP('',(#3281));
#787=EDGE_LOOP('',(#3282,#3283,#3284,#3285));
#788=EDGE_LOOP('',(#3286));
#789=EDGE_LOOP('',(#3287));
#790=EDGE_LOOP('',(#3288,#3289,#3290,#3291));
#791=EDGE_LOOP('',(#3292,#3293,#3294,#3295));
#792=EDGE_LOOP('',(#3296));
#793=EDGE_LOOP('',(#3297));
#794=EDGE_LOOP('',(#3298,#3299,#3300,#3301));
#795=EDGE_LOOP('',(#3302,#3303,#3304,#3305));
#796=EDGE_LOOP('',(#3306,#3307,#3308,#3309));
#797=EDGE_LOOP('',(#3310));
#798=EDGE_LOOP('',(#3311));
#799=EDGE_LOOP('',(#3312,#3313,#3314,#3315));
#800=EDGE_LOOP('',(#3316,#3317,#3318,#3319));
#801=EDGE_LOOP('',(#3320));
#802=EDGE_LOOP('',(#3321));
#803=EDGE_LOOP('',(#3322,#3323,#3324,#3325));
#804=EDGE_LOOP('',(#3326,#3327,#3328,#3329));
#805=EDGE_LOOP('',(#3330,#3331,#3332,#3333));
#806=EDGE_LOOP('',(#3334,#3335,#3336,#3337));
#807=EDGE_LOOP('',(#3338,#3339,#3340,#3341));
#808=EDGE_LOOP('',(#3342,#3343,#3344,#3345));
#809=EDGE_LOOP('',(#3346,#3347,#3348,#3349));
#810=EDGE_LOOP('',(#3350,#3351,#3352,#3353));
#811=EDGE_LOOP('',(#3354,#3355,#3356,#3357));
#812=EDGE_LOOP('',(#3358,#3359,#3360,#3361));
#813=EDGE_LOOP('',(#3362,#3363,#3364,#3365,#3366,#3367));
#814=EDGE_LOOP('',(#3368,#3369,#3370,#3371));
#815=EDGE_LOOP('',(#3372,#3373,#3374,#3375,#3376,#3377));
#816=EDGE_LOOP('',(#3378,#3379,#3380,#3381));
#817=EDGE_LOOP('',(#3382,#3383,#3384,#3385));
#818=EDGE_LOOP('',(#3386,#3387,#3388,#3389));
#819=EDGE_LOOP('',(#3390,#3391));
#820=EDGE_LOOP('',(#3392,#3393));
#821=LINE('',#4942,#979);
#822=LINE('',#4984,#980);
#823=LINE('',#4993,#981);
#824=LINE('',#4998,#982);
#825=LINE('',#5001,#983);
#826=LINE('',#5006,#984);
#827=LINE('',#5010,#985);
#828=LINE('',#5013,#986);
#829=LINE('',#5018,#987);
#830=LINE('',#5022,#988);
#831=LINE('',#5026,#989);
#832=LINE('',#5033,#990);
#833=LINE('',#5040,#991);
#834=LINE('',#5044,#992);
#835=LINE('',#5048,#993);
#836=LINE('',#5052,#994);
#837=LINE('',#5056,#995);
#838=LINE('',#5063,#996);
#839=LINE('',#5068,#997);
#840=LINE('',#5074,#998);
#841=LINE('',#5346,#999);
#842=LINE('',#5736,#1000);
#843=LINE('',#5862,#1001);
#844=LINE('',#6173,#1002);
#845=LINE('',#6561,#1003);
#846=LINE('',#6960,#1004);
#847=LINE('',#7347,#1005);
#848=LINE('',#7748,#1006);
#849=LINE('',#8143,#1007);
#850=LINE('',#8552,#1008);
#851=LINE('',#8955,#1009);
#852=LINE('',#9337,#1010);
#853=LINE('',#14357,#1011);
#854=LINE('',#15429,#1012);
#855=LINE('',#15440,#1013);
#856=LINE('',#15458,#1014);
#857=LINE('',#15471,#1015);
#858=LINE('',#15488,#1016);
#859=LINE('',#15508,#1017);
#860=LINE('',#15510,#1018);
#861=LINE('',#15512,#1019);
#862=LINE('',#15559,#1020);
#863=LINE('',#15575,#1021);
#864=LINE('',#15581,#1022);
#865=LINE('',#15640,#1023);
#866=LINE('',#15647,#1024);
#867=LINE('',#15649,#1025);
#868=LINE('',#15651,#1026);
#869=LINE('',#15652,#1027);
#870=LINE('',#15655,#1028);
#871=LINE('',#15657,#1029);
#872=LINE('',#15658,#1030);
#873=LINE('',#15661,#1031);
#874=LINE('',#15663,#1032);
#875=LINE('',#15664,#1033);
#876=LINE('',#15667,#1034);
#877=LINE('',#15669,#1035);
#878=LINE('',#15670,#1036);
#879=LINE('',#15673,#1037);
#880=LINE('',#15675,#1038);
#881=LINE('',#15676,#1039);
#882=LINE('',#15678,#1040);
#883=LINE('',#15679,#1041);
#884=LINE('',#15686,#1042);
#885=LINE('',#15959,#1043);
#886=LINE('',#16352,#1044);
#887=LINE('',#16711,#1045);
#888=LINE('',#17052,#1046);
#889=LINE('',#17395,#1047);
#890=LINE('',#21327,#1048);
#891=LINE('',#22114,#1049);
#892=LINE('',#22128,#1050);
#893=LINE('',#22145,#1051);
#894=LINE('',#22166,#1052);
#895=LINE('',#22175,#1053);
#896=LINE('',#22186,#1054);
#897=LINE('',#22197,#1055);
#898=LINE('',#22208,#1056);
#899=LINE('',#22219,#1057);
#900=LINE('',#22230,#1058);
#901=LINE('',#22241,#1059);
#902=LINE('',#22252,#1060);
#903=LINE('',#22263,#1061);
#904=LINE('',#22274,#1062);
#905=LINE('',#22285,#1063);
#906=LINE('',#22296,#1064);
#907=LINE('',#22307,#1065);
#908=LINE('',#22309,#1066);
#909=LINE('',#22318,#1067);
#910=LINE('',#22329,#1068);
#911=LINE('',#22340,#1069);
#912=LINE('',#22351,#1070);
#913=LINE('',#22362,#1071);
#914=LINE('',#22373,#1072);
#915=LINE('',#22384,#1073);
#916=LINE('',#22395,#1074);
#917=LINE('',#22406,#1075);
#918=LINE('',#22417,#1076);
#919=LINE('',#22428,#1077);
#920=LINE('',#22439,#1078);
#921=LINE('',#22449,#1079);
#922=LINE('',#22460,#1080);
#923=LINE('',#22471,#1081);
#924=LINE('',#22482,#1082);
#925=LINE('',#22493,#1083);
#926=LINE('',#22504,#1084);
#927=LINE('',#22515,#1085);
#928=LINE('',#22526,#1086);
#929=LINE('',#22537,#1087);
#930=LINE('',#22548,#1088);
#931=LINE('',#22559,#1089);
#932=LINE('',#22570,#1090);
#933=LINE('',#22581,#1091);
#934=LINE('',#22592,#1092);
#935=LINE('',#22594,#1093);
#936=LINE('',#22603,#1094);
#937=LINE('',#22614,#1095);
#938=LINE('',#22625,#1096);
#939=LINE('',#22636,#1097);
#940=LINE('',#22647,#1098);
#941=LINE('',#22658,#1099);
#942=LINE('',#22669,#1100);
#943=LINE('',#22680,#1101);
#944=LINE('',#22691,#1102);
#945=LINE('',#22702,#1103);
#946=LINE('',#22713,#1104);
#947=LINE('',#22724,#1105);
#948=LINE('',#22735,#1106);
#949=LINE('',#22745,#1107);
#950=LINE('',#25657,#1108);
#951=LINE('',#25666,#1109);
#952=LINE('',#25683,#1110);
#953=LINE('',#25688,#1111);
#954=LINE('',#25694,#1112);
#955=LINE('',#25700,#1113);
#956=LINE('',#25703,#1114);
#957=LINE('',#25752,#1115);
#958=LINE('',#25768,#1116);
#959=LINE('',#25774,#1117);
#960=LINE('',#25833,#1118);
#961=LINE('',#25840,#1119);
#962=LINE('',#25842,#1120);
#963=LINE('',#25844,#1121);
#964=LINE('',#25845,#1122);
#965=LINE('',#25848,#1123);
#966=LINE('',#25850,#1124);
#967=LINE('',#25851,#1125);
#968=LINE('',#25854,#1126);
#969=LINE('',#25856,#1127);
#970=LINE('',#25857,#1128);
#971=LINE('',#25860,#1129);
#972=LINE('',#25862,#1130);
#973=LINE('',#25863,#1131);
#974=LINE('',#25866,#1132);
#975=LINE('',#25868,#1133);
#976=LINE('',#25869,#1134);
#977=LINE('',#25871,#1135);
#978=LINE('',#25872,#1136);
#979=VECTOR('',#4120,0.999999999999999);
#980=VECTOR('',#4125,5.);
#981=VECTOR('',#4136,7.20746054905241);
#982=VECTOR('',#4143,7.52312685038423);
#983=VECTOR('',#4146,7.36529369971832);
#984=VECTOR('',#4153,7.36790580323689);
#985=VECTOR('',#4158,7.52835105742136);
#986=VECTOR('',#4161,6.97561584944256);
#987=VECTOR('',#4168,6.41628586403442);
#988=VECTOR('',#4173,6.40969108660508);
#989=VECTOR('',#4178,6.40906719549494);
#990=VECTOR('',#4187,6.41550316824698);
#991=VECTOR('',#4196,6.40820475053297);
#992=VECTOR('',#4201,6.40787078036307);
#993=VECTOR('',#4206,6.40732538114918);
#994=VECTOR('',#4211,6.40706623219228);
#995=VECTOR('',#4216,6.40667124022599);
#996=VECTOR('',#4225,4.66385643997278);
#997=VECTOR('',#4232,3.44589712386029);
#998=VECTOR('',#4239,1.77625);
#999=VECTOR('',#4244,1.77625);
#1000=VECTOR('',#4247,1.77625);
#1001=VECTOR('',#4250,1.77625);
#1002=VECTOR('',#4253,1.77625);
#1003=VECTOR('',#4256,1.77625);
#1004=VECTOR('',#4259,1.77625);
#1005=VECTOR('',#4262,1.77625);
#1006=VECTOR('',#4265,1.77625);
#1007=VECTOR('',#4268,1.77625);
#1008=VECTOR('',#4271,1.77625);
#1009=VECTOR('',#4274,1.77625);
#1010=VECTOR('',#4277,1.77625);
#1011=VECTOR('',#4306,6.40820475053297);
#1012=VECTOR('',#4331,4.48902817623056);
#1013=VECTOR('',#4346,6.40950758978419);
#1014=VECTOR('',#4371,6.40867450936473);
#1015=VECTOR('',#4390,6.40772765523458);
#1016=VECTOR('',#4413,6.40690599146347);
#1017=VECTOR('',#4442,4.42329516333974);
#1018=VECTOR('',#4445,2.21164758166987);
#1019=VECTOR('',#4448,2.21164758166987);
#1020=VECTOR('',#4451,10.);
#1021=VECTOR('',#4452,10.);
#1022=VECTOR('',#4459,10.);
#1023=VECTOR('',#4460,10.);
#1024=VECTOR('',#4469,10.);
#1025=VECTOR('',#4470,10.);
#1026=VECTOR('',#4471,10.);
#1027=VECTOR('',#4472,10.);
#1028=VECTOR('',#4475,9.99999999999999);
#1029=VECTOR('',#4476,9.99999999999999);
#1030=VECTOR('',#4477,10.);
#1031=VECTOR('',#4480,10.);
#1032=VECTOR('',#4481,10.);
#1033=VECTOR('',#4482,10.);
#1034=VECTOR('',#4485,10.);
#1035=VECTOR('',#4486,10.);
#1036=VECTOR('',#4487,10.);
#1037=VECTOR('',#4490,10.);
#1038=VECTOR('',#4491,10.);
#1039=VECTOR('',#4492,10.);
#1040=VECTOR('',#4495,10.);
#1041=VECTOR('',#4496,10.);
#1042=VECTOR('',#4505,3.72275);
#1043=VECTOR('',#4510,3.72275);
#1044=VECTOR('',#4513,3.72275);
#1045=VECTOR('',#4516,3.72275);
#1046=VECTOR('',#4519,3.72275);
#1047=VECTOR('',#4522,3.72275);
#1048=VECTOR('',#4549,2.204);
#1049=VECTOR('',#4556,5.42440960677665);
#1050=VECTOR('',#4577,6.40906719549494);
#1051=VECTOR('',#4602,6.40732538114918);
#1052=VECTOR('',#4619,10.);
#1053=VECTOR('',#4620,10.);
#1054=VECTOR('',#4621,10.);
#1055=VECTOR('',#4622,10.);
#1056=VECTOR('',#4623,10.);
#1057=VECTOR('',#4624,10.);
#1058=VECTOR('',#4625,10.);
#1059=VECTOR('',#4626,10.);
#1060=VECTOR('',#4627,10.);
#1061=VECTOR('',#4628,10.);
#1062=VECTOR('',#4629,10.);
#1063=VECTOR('',#4630,10.);
#1064=VECTOR('',#4631,10.);
#1065=VECTOR('',#4632,10.);
#1066=VECTOR('',#4633,10.);
#1067=VECTOR('',#4634,10.);
#1068=VECTOR('',#4635,10.);
#1069=VECTOR('',#4636,10.);
#1070=VECTOR('',#4637,10.);
#1071=VECTOR('',#4638,10.);
#1072=VECTOR('',#4639,10.);
#1073=VECTOR('',#4640,10.);
#1074=VECTOR('',#4641,10.);
#1075=VECTOR('',#4642,10.);
#1076=VECTOR('',#4643,10.);
#1077=VECTOR('',#4644,10.);
#1078=VECTOR('',#4645,10.);
#1079=VECTOR('',#4646,10.);
#1080=VECTOR('',#4649,10.);
#1081=VECTOR('',#4650,10.);
#1082=VECTOR('',#4651,10.);
#1083=VECTOR('',#4652,10.);
#1084=VECTOR('',#4653,10.);
#1085=VECTOR('',#4654,10.);
#1086=VECTOR('',#4655,10.);
#1087=VECTOR('',#4656,10.);
#1088=VECTOR('',#4657,10.);
#1089=VECTOR('',#4658,10.);
#1090=VECTOR('',#4659,10.);
#1091=VECTOR('',#4660,10.);
#1092=VECTOR('',#4661,10.);
#1093=VECTOR('',#4662,10.);
#1094=VECTOR('',#4663,10.);
#1095=VECTOR('',#4664,10.);
#1096=VECTOR('',#4665,10.);
#1097=VECTOR('',#4666,10.);
#1098=VECTOR('',#4667,10.);
#1099=VECTOR('',#4668,10.);
#1100=VECTOR('',#4669,10.);
#1101=VECTOR('',#4670,10.);
#1102=VECTOR('',#4671,10.);
#1103=VECTOR('',#4672,10.);
#1104=VECTOR('',#4673,10.);
#1105=VECTOR('',#4674,10.);
#1106=VECTOR('',#4675,10.);
#1107=VECTOR('',#4676,10.);
#1108=VECTOR('',#4755,5.);
#1109=VECTOR('',#4768,4.88180150972878);
#1110=VECTOR('',#4793,4.88180150972878);
#1111=VECTOR('',#4798,2.204);
#1112=VECTOR('',#4805,6.97561584944256);
#1113=VECTOR('',#4814,7.52835105742136);
#1114=VECTOR('',#4817,6.97638033209901);
#1115=VECTOR('',#4824,10.);
#1116=VECTOR('',#4825,10.);
#1117=VECTOR('',#4832,10.);
#1118=VECTOR('',#4833,10.);
#1119=VECTOR('',#4842,10.);
#1120=VECTOR('',#4843,10.);
#1121=VECTOR('',#4844,10.);
#1122=VECTOR('',#4845,10.);
#1123=VECTOR('',#4848,9.99999999999999);
#1124=VECTOR('',#4849,9.99999999999999);
#1125=VECTOR('',#4850,10.);
#1126=VECTOR('',#4853,10.);
#1127=VECTOR('',#4854,10.);
#1128=VECTOR('',#4855,10.);
#1129=VECTOR('',#4858,10.);
#1130=VECTOR('',#4859,10.);
#1131=VECTOR('',#4860,10.);
#1132=VECTOR('',#4863,10.);
#1133=VECTOR('',#4864,10.);
#1134=VECTOR('',#4865,10.);
#1135=VECTOR('',#4868,10.);
#1136=VECTOR('',#4869,10.);
#1137=B_SPLINE_CURVE_WITH_KNOTS('',3,(#4905,#4906,#4907,#4908,#4909,#4910,
#4911,#4912,#4913,#4914,#4915,#4916,#4917,#4918,#4919,#4920,#4921,#4922,
#4923,#4924,#4925,#4926,#4927,#4928,#4929,#4930),.UNSPECIFIED.,.F.,.F.,
(4,2,2,2,2,2,2,2,2,2,2,2,4),(-0.606481282784619,-0.568571286664201,-0.530661290543783,
-0.492761126316124,-0.454860962088464,-0.416960797860805,-0.379060633633146,
-0.341150637512728,-0.30324064139231,-0.265330645271891,-0.227420649151473,
-0.189520484923814,-0.151620320696155),.UNSPECIFIED.);
#1138=B_SPLINE_CURVE_WITH_KNOTS('',3,(#4931,#4932,#4933,#4934,#4935,#4936,
#4937,#4938,#4939,#4940),.UNSPECIFIED.,.F.,.F.,(4,2,2,2,4),(-0.151620320696155,
-0.113720156468496,-0.0758199922408364,-0.0379099961204182,0.),
 .UNSPECIFIED.);
#1139=B_SPLINE_CURVE_WITH_KNOTS('',3,(#4944,#4945,#4946,#4947,#4948,#4949,
#4950,#4951,#4952,#4953),.UNSPECIFIED.,.F.,.F.,(4,2,2,2,4),(0.,0.0377168406459521,
0.0754336812919042,0.113150118256495,0.150866555221085),.UNSPECIFIED.);
#1140=B_SPLINE_CURVE_WITH_KNOTS('',3,(#4954,#4955,#4956,#4957,#4958,#4959,
#4960,#4961,#4962,#4963,#4964,#4965,#4966,#4967,#4968,#4969,#4970,#4971,
#4972,#4973,#4974,#4975,#4976,#4977,#4978,#4979),.UNSPECIFIED.,.F.,.F.,
(4,2,2,2,2,2,2,2,2,2,2,2,4),(0.150866555221085,0.188582992185676,0.226299429150267,
0.264016269796219,0.301733110442171,0.339449951088123,0.377166791734075,
0.414883228698666,0.452599665663256,0.490316102627847,0.528032539592437,
0.565749380238389,0.603466220884342),.UNSPECIFIED.);
#1141=B_SPLINE_CURVE_WITH_KNOTS('',3,(#5076,#5077,#5078,#5079,#5080,#5081,
#5082,#5083,#5084,#5085,#5086,#5087,#5088,#5089,#5090,#5091,#5092,#5093,
#5094,#5095,#5096,#5097,#5098,#5099,#5100,#5101,#5102,#5103,#5104,#5105,
#5106,#5107,#5108,#5109,#5110,#5111,#5112,#5113,#5114,#5115,#5116,#5117,
#5118,#5119,#5120,#5121,#5122,#5123,#5124,#5125,#5126,#5127,#5128,#5129,
#5130,#5131,#5132,#5133,#5134,#5135,#5136,#5137,#5138,#5139,#5140,#5141,
#5142,#5143,#5144,#5145,#5146,#5147,#5148,#5149,#5150,#5151,#5152,#5153,
#5154,#5155,#5156,#5157,#5158,#5159,#5160,#5161,#5162,#5163,#5164,#5165,
#5166,#5167,#5168,#5169,#5170,#5171,#5172,#5173,#5174,#5175,#5176,#5177,
#5178,#5179,#5180,#5181,#5182,#5183,#5184,#5185,#5186,#5187,#5188,#5189,
#5190,#5191,#5192,#5193,#5194,#5195,#5196,#5197,#5198,#5199,#5200,#5201,
#5202,#5203,#5204,#5205,#5206,#5207,#5208,#5209,#5210,#5211,#5212,#5213,
#5214,#5215,#5216,#5217,#5218,#5219,#5220,#5221,#5222,#5223),
 .UNSPECIFIED.,.F.,.F.,(4,2,2,2,2,2,2,2,2,2,2,2,2,2,2,2,2,2,2,2,2,2,2,2,
2,2,2,2,2,2,2,2,2,2,2,2,2,2,2,2,2,2,2,2,2,2,2,2,2,2,2,2,2,2,2,2,2,2,2,2,
2,2,2,2,2,2,2,2,2,2,2,2,2,4),(-0.835356566537246,-0.834179578002919,-0.832057305629885,
-0.82934175770569,-0.823544728796445,-0.815449054574031,-0.790979904521206,
-0.758630520976316,-0.751247845401951,-0.746562671739766,-0.7427957472337,
-0.738457675321842,-0.730730673891037,-0.705406951032464,-0.667022076483651,
-0.660027153413853,-0.657302375275477,-0.655127611169892,-0.652797944555009,
-0.648926745100182,-0.632840827180127,-0.581115393054966,-0.57367752973655,
-0.568973506689807,-0.565200732382815,-0.560865809230101,-0.55317110435513,
-0.528123923872481,-0.491328745297315,-0.482817000286532,-0.479581086366103,
-0.477413245958042,-0.475106128977813,-0.471268591582215,-0.455353920220774,
-0.406196234245469,-0.39585526201539,-0.391035642446638,-0.38727899810539,
-0.3830778783461,-0.375924745588849,-0.367161529927778,-0.347550182457797,
-0.318343151462567,-0.305702905197989,-0.302000513660807,-0.299719364921067,
-0.297497437811916,-0.294122055897232,-0.283819597360589,-0.265015419181205,
-0.224003622448924,-0.216331810091993,-0.211947796786676,-0.20854279480949,
-0.204038955946528,-0.195556237330191,-0.184620571805917,-0.155613520886967,
-0.130863977628998,-0.12539325974147,-0.12272421983817,-0.12056335417637,
-0.117801735198089,-0.111949409671634,-0.0861381627528235,-0.0532557845040427,
-0.0423421159714301,-0.0374256406153841,-0.0335867130961813,-0.0300163926963186,
-0.0258468770318152,-0.0165211006533095,-0.000528019587408642),
 .UNSPECIFIED.);
#1142=B_SPLINE_CURVE_WITH_KNOTS('',3,(#5225,#5226,#5227,#5228,#5229,#5230,
#5231),.UNSPECIFIED.,.F.,.F.,(4,3,4),(15.4636264665944,15.5857948670228,
15.7079632674512),.UNSPECIFIED.);
#1143=B_SPLINE_CURVE_WITH_KNOTS('',3,(#5234,#5235,#5236,#5237,#5238,#5239,
#5240,#5241,#5242,#5243,#5244,#5245,#5246,#5247,#5248,#5249,#5250,#5251,
#5252,#5253,#5254,#5255,#5256,#5257,#5258,#5259,#5260,#5261,#5262,#5263,
#5264,#5265,#5266,#5267,#5268,#5269,#5270,#5271,#5272,#5273,#5274,#5275,
#5276,#5277,#5278,#5279,#5280,#5281,#5282,#5283,#5284,#5285,#5286,#5287,
#5288,#5289,#5290,#5291,#5292,#5293,#5294,#5295,#5296,#5297,#5298,#5299,
#5300,#5301,#5302,#5303,#5304,#5305,#5306,#5307,#5308,#5309,#5310,#5311,
#5312,#5313,#5314,#5315,#5316,#5317,#5318,#5319,#5320,#5321,#5322,#5323,
#5324,#5325,#5326,#5327,#5328,#5329,#5330,#5331,#5332,#5333,#5334,#5335,
#5336,#5337,#5338,#5339,#5340,#5341,#5342),.UNSPECIFIED.,.F.,.F.,(4,3,3,
3,3,3,3,3,3,3,3,3,3,3,3,3,3,3,3,3,3,3,3,3,3,3,3,3,3,3,3,3,3,3,3,3,4),(16.7019922841306,
16.8124544772726,16.9234210411684,17.033796869599,17.1441744311209,17.2545854631975,
17.3659858445079,17.4766375907132,17.5884122895762,17.7001869884391,17.8072802155964,
17.9186679002403,18.0254288144202,18.1321132984658,18.2387615669814,18.3454137772225,
18.4521802784855,18.5590147146697,18.6660336585631,18.6983816927476,18.8065090728564,
18.9177674883813,19.025595407644,19.1333563054358,19.2410888397907,19.3488316227747,
19.4566913005886,19.5646218816293,19.6727314597256,19.6965763970561,19.8047706499335,
19.912813978709,20.0207451306855,20.1286177204737,20.2364557658273,20.3443346961532,
20.3930532338378),.UNSPECIFIED.);
#1144=B_SPLINE_CURVE_WITH_KNOTS('',3,(#5347,#5348,#5349,#5350,#5351,#5352,
#5353,#5354,#5355,#5356,#5357,#5358,#5359,#5360,#5361,#5362,#5363,#5364,
#5365,#5366,#5367,#5368,#5369,#5370,#5371,#5372,#5373,#5374,#5375,#5376,
#5377,#5378,#5379,#5380,#5381,#5382,#5383,#5384,#5385,#5386,#5387,#5388,
#5389,#5390,#5391,#5392,#5393,#5394,#5395,#5396,#5397,#5398,#5399,#5400,
#5401,#5402,#5403,#5404,#5405,#5406,#5407,#5408,#5409,#5410,#5411,#5412,
#5413,#5414,#5415,#5416,#5417,#5418,#5419,#5420,#5421,#5422,#5423,#5424,
#5425,#5426,#5427,#5428,#5429,#5430,#5431,#5432,#5433,#5434,#5435,#5436,
#5437,#5438,#5439,#5440,#5441,#5442,#5443,#5444,#5445,#5446,#5447,#5448,
#5449,#5450,#5451,#5452,#5453,#5454,#5455,#5456,#5457,#5458,#5459,#5460,
#5461,#5462,#5463,#5464,#5465,#5466,#5467,#5468,#5469,#5470,#5471,#5472,
#5473,#5474,#5475,#5476,#5477,#5478,#5479,#5480,#5481,#5482,#5483,#5484,
#5485,#5486,#5487,#5488,#5489,#5490,#5491,#5492,#5493,#5494,#5495,#5496,
#5497,#5498,#5499,#5500,#5501,#5502,#5503,#5504,#5505,#5506,#5507,#5508,
#5509,#5510,#5511,#5512,#5513,#5514,#5515,#5516,#5517,#5518,#5519,#5520,
#5521,#5522,#5523,#5524,#5525,#5526,#5527,#5528,#5529,#5530,#5531,#5532,
#5533,#5534,#5535,#5536,#5537,#5538,#5539,#5540),.UNSPECIFIED.,.F.,.F.,
(4,2,2,2,2,2,2,2,2,2,2,2,2,2,2,2,2,2,2,2,2,2,2,2,2,2,2,2,2,2,2,2,2,2,2,
2,2,2,2,2,2,2,2,2,2,2,2,2,2,2,2,2,2,2,2,2,2,2,2,2,2,2,2,2,2,2,2,2,2,2,2,
2,2,2,2,2,2,2,2,2,2,2,2,2,2,2,2,2,2,2,2,2,2,2,2,2,4),(-1.95454507750439,
-1.92969887688555,-1.90700587487671,-1.90284449273311,-1.90045698570642,
-1.89829258749123,-1.89520508387779,-1.88936360059004,-1.85017890081121,
-1.82470793213726,-1.81696215744342,-1.81262184818882,-1.80885764965132,
-1.80418199299687,-1.79682683246125,-1.76279416764177,-1.73956966484566,
-1.73169570283323,-1.72601764868932,-1.72332439775519,-1.72120226710614,
-1.71856614706167,-1.7131897934261,-1.68420858229177,-1.66980886534623,
-1.65294595377729,-1.64134625560956,-1.63629734544878,-1.63249199363362,
-1.62836280128111,-1.62163051869468,-1.59092369606964,-1.5680581423284,
-1.55098317581711,-1.54705937226041,-1.54472310228857,-1.54256020421295,
-1.53987248019897,-1.53309414208251,-1.49446663046274,-1.46909648525411,
-1.46136459634652,-1.45702729073491,-1.45326306026007,-1.44858395184908,
-1.44121641047095,-1.40788434579373,-1.3841471969067,-1.37618087956058,
-1.37045355392296,-1.3677512422959,-1.36562903738565,-1.3630016479163,-1.35767008544244,
-1.3177711925292,-1.29148760005246,-1.28363221952914,-1.27926932868241,
-1.27550681445262,-1.27086060774184,-1.26360717745568,-1.22625306573836,
-1.2053446946898,-1.19438739470466,-1.19094604449721,-1.18871382456224,
-1.18643941074527,-1.18280332363237,-1.17100933713551,-1.13755203671263,
-1.12000271682831,-1.10834732008514,-1.10366159282688,-1.09980654930369,
-1.09585161550517,-1.08996582836221,-1.07189826280532,-1.03983979736194,
-1.01808202486886,-1.01388329213852,-1.01148758987828,-1.00932756295218,
-1.00626130276856,-0.998311944972997,-0.985704858969611,-0.961762341328657,
-0.933727639097285,-0.927057916080415,-0.922943834088199,-0.919137263230214,
-0.914064099371912,-0.902299995493179,-0.885082792620805,-0.873876918369987,
-0.842062810475459,-0.836793926929779,-0.835356566537246),.UNSPECIFIED.);
#1145=B_SPLINE_CURVE_WITH_KNOTS('',3,(#5542,#5543,#5544,#5545,#5546,#5547,
#5548,#5549,#5550,#5551,#5552,#5553,#5554,#5555,#5556,#5557,#5558,#5559,
#5560,#5561,#5562,#5563,#5564,#5565,#5566,#5567,#5568,#5569,#5570,#5571,
#5572,#5573,#5574,#5575,#5576,#5577,#5578,#5579,#5580,#5581,#5582,#5583,
#5584,#5585,#5586,#5587,#5588,#5589,#5590),.UNSPECIFIED.,.F.,.F.,(4,3,3,
3,3,3,3,3,3,3,3,3,3,3,3,3,4),(20.3930532338378,20.5010566943853,20.6092613750708,
20.6947711013646,20.8026970972416,20.9139806857955,21.0216059003609,21.1291641701826,
21.2366944839657,21.3442357847572,21.4518963786598,21.5596290516459,21.6675442181706,
21.6929658056731,21.8250574021607,21.9552551911513,21.9911485745994),
 .UNSPECIFIED.);
#1146=B_SPLINE_CURVE_WITH_KNOTS('',3,(#5591,#5592,#5593,#5594,#5595,#5596,
#5597,#5598,#5599,#5600,#5601,#5602,#5603,#5604,#5605,#5606,#5607,#5608,
#5609,#5610,#5611,#5612,#5613,#5614,#5615,#5616,#5617,#5618,#5619,#5620,
#5621,#5622,#5623,#5624,#5625,#5626,#5627,#5628,#5629,#5630,#5631,#5632,
#5633,#5634,#5635,#5636,#5637,#5638,#5639,#5640,#5641,#5642,#5643,#5644,
#5645,#5646,#5647,#5648,#5649,#5650,#5651,#5652,#5653,#5654,#5655,#5656,
#5657,#5658,#5659,#5660,#5661,#5662,#5663,#5664,#5665,#5666,#5667,#5668,
#5669,#5670,#5671,#5672,#5673,#5674,#5675,#5676,#5677,#5678,#5679,#5680,
#5681,#5682,#5683,#5684,#5685,#5686,#5687,#5688,#5689,#5690,#5691,#5692,
#5693,#5694,#5695,#5696,#5697,#5698,#5699,#5700,#5701,#5702,#5703,#5704,
#5705,#5706,#5707,#5708,#5709,#5710,#5711,#5712,#5713,#5714,#5715,#5716,
#5717,#5718,#5719,#5720,#5721,#5722,#5723,#5724,#5725,#5726,#5727,#5728,
#5729,#5730,#5731,#5732),.UNSPECIFIED.,.F.,.F.,(4,3,3,3,3,3,3,3,3,3,3,3,
3,3,3,3,3,3,3,3,3,3,3,3,3,3,3,3,3,3,3,3,3,3,3,3,3,3,3,3,3,3,3,3,3,3,3,4),
(21.9911485751285,22.0981765274336,22.2051623507136,22.3121457608551,22.4192405673634,
22.5263967550779,22.6337465274261,22.6911605099816,22.7992205091258,22.9104873472713,
23.0182513855477,23.1259498862704,23.2336216180078,23.3413053050867,23.4491088121582,
23.5569848760485,23.6650428436122,23.6893552142901,23.7973810979624,23.9086522005419,
24.0163805862326,24.1240429630528,24.2316781568489,24.3393249487448,24.4470912677292,
24.5549299286194,24.6629505155869,24.6875499185986,24.7955941221079,24.9068629347078,
25.0146102076539,25.1222916298659,25.2299459967969,25.3376120593305,25.4453976697339,
25.5532556566589,25.6612954465704,25.6857446229071,25.7937879777517,25.904155195045,
26.0119016507377,26.1195817394621,26.2272342594645,26.3396071236228,26.4473901517118,
26.5552467306643,26.6632787454227,26.6767257160977),.UNSPECIFIED.);
#1147=B_SPLINE_CURVE_WITH_KNOTS('',3,(#5738,#5739,#5740,#5741,#5742,#5743,
#5744,#5745,#5746),.UNSPECIFIED.,.F.,.F.,(4,1,1,1,1,1,4),(28.274333882308,
28.3671761734046,29.365370877713,30.3635655820215,31.36176028633,32.3599549906385,
32.9594405895371),.UNSPECIFIED.);
#1148=B_SPLINE_CURVE_WITH_KNOTS('',3,(#5747,#5748,#5749,#5750,#5751,#5752,
#5753,#5754,#5755,#5756,#5757,#5758,#5759,#5760,#5761,#5762,#5763,#5764,
#5765,#5766,#5767,#5768,#5769,#5770,#5771,#5772,#5773,#5774,#5775,#5776,
#5777,#5778,#5779,#5780,#5781,#5782,#5783,#5784,#5785,#5786,#5787,#5788,
#5789,#5790,#5791,#5792,#5793,#5794,#5795,#5796),.UNSPECIFIED.,.F.,.F.,
(4,2,2,2,2,2,2,2,2,2,2,2,2,2,2,2,2,2,2,2,2,2,2,2,4),(-2.23915986394093,
-2.20592704873654,-2.18032577745133,-2.17256259015734,-2.16821888680587,
-2.16445526260495,-2.15978487840366,-2.15244732829037,-2.1175945351571,
-2.09496188142004,-2.08719720497901,-2.08157791702537,-2.07889578751457,
-2.07677406554045,-2.0741280407893,-2.06869901710893,-2.04323247885477,
-2.02010812726836,-1.99943956922362,-1.99331541844904,-1.98931322858529,
-1.98549354859668,-1.98011485708538,-1.96718673212748,-1.95454507750439),
 .UNSPECIFIED.);
#1149=B_SPLINE_CURVE_WITH_KNOTS('',3,(#5798,#5799,#5800,#5801,#5802,#5803,
#5804,#5805,#5806,#5807,#5808,#5809,#5810,#5811,#5812,#5813,#5814,#5815,
#5816,#5817,#5818,#5819,#5820,#5821,#5822,#5823,#5824,#5825,#5826,#5827,
#5828,#5829,#5830,#5831,#5832,#5833,#5834,#5835,#5836,#5837,#5838,#5839,
#5840,#5841,#5842,#5843,#5844,#5845,#5846,#5847,#5848,#5849),
 .UNSPECIFIED.,.F.,.F.,(4,3,3,3,3,3,3,3,3,3,3,3,3,3,3,3,3,4),(26.6767257160977,
26.6839393272156,26.7919782863231,26.9032477544733,27.0109896752984,27.1186657202993,
27.2263146935872,27.3339753546827,27.4417555868768,27.5496082029795,27.6576426811105,
27.6821340315241,27.7919683102848,27.9016171368834,28.0110886501516,28.1204564526687,
28.2297536032295,28.274333882308),.UNSPECIFIED.);
#1150=B_SPLINE_CURVE_WITH_KNOTS('',3,(#5850,#5851,#5852,#5853,#5854,#5855,
#5856,#5857,#5858),.UNSPECIFIED.,.F.,.F.,(4,1,1,1,1,1,4),(28.2743402347403,
28.6803287358326,29.6785234401411,30.6767181444496,31.6749128487581,32.6731075530666,
32.9608271762519),.UNSPECIFIED.);
#1151=B_SPLINE_CURVE_WITH_KNOTS('',3,(#5864,#5865,#5866,#5867,#5868,#5869,
#5870,#5871,#5872,#5873,#5874,#5875,#5876,#5877,#5878,#5879,#5880,#5881,
#5882,#5883,#5884,#5885,#5886,#5887,#5888,#5889,#5890,#5891,#5892,#5893,
#5894,#5895,#5896,#5897,#5898,#5899,#5900,#5901,#5902,#5903,#5904,#5905,
#5906,#5907,#5908,#5909,#5910,#5911,#5912,#5913,#5914,#5915,#5916,#5917,
#5918,#5919,#5920,#5921,#5922,#5923,#5924,#5925,#5926,#5927,#5928,#5929,
#5930,#5931,#5932,#5933,#5934,#5935,#5936,#5937,#5938,#5939,#5940,#5941,
#5942,#5943,#5944,#5945,#5946,#5947,#5948,#5949,#5950,#5951,#5952,#5953,
#5954,#5955,#5956,#5957,#5958,#5959,#5960,#5961,#5962,#5963,#5964,#5965,
#5966,#5967,#5968,#5969,#5970,#5971,#5972,#5973,#5974,#5975,#5976,#5977,
#5978,#5979,#5980,#5981,#5982,#5983,#5984,#5985,#5986,#5987,#5988,#5989,
#5990,#5991,#5992,#5993,#5994,#5995,#5996,#5997,#5998,#5999,#6000,#6001,
#6002,#6003,#6004,#6005),.UNSPECIFIED.,.F.,.F.,(4,3,3,3,3,3,3,3,3,3,3,3,
3,3,3,3,3,3,3,3,3,3,3,3,3,3,3,3,3,3,3,3,3,3,3,3,3,3,3,3,3,3,3,3,3,3,3,4),
(34.5575193977698,34.6637962689209,34.7699803795124,34.8761126116981,34.9822337650756,
35.088455256206,35.194732459932,35.3011944966565,35.354539103564,35.4625799721229,
35.5738492015916,35.681593103219,35.7892711499964,35.8969221428487,36.0045848381315,
36.112367113131,36.2202217794645,36.3282583002447,36.3527338078725,36.4607746770588,
36.5720439064491,36.6797878087295,36.7874658561678,36.8951168496875,37.0027795456435,
37.1105618213201,37.2184164883337,37.3264530097926,37.350928512181,37.4589693811155,
37.5702386105372,37.6779825125593,37.7856605597373,37.8933115529956,38.000974248689,
38.1087565241035,38.216611190855,38.324647712054,38.3491232164895,38.4608178024709,
38.568667102327,38.6764084850113,38.7840808451954,38.8917229858393,38.9994241461165,
39.1071616534688,39.2150320522313,39.2426799043403),.UNSPECIFIED.);
#1152=B_SPLINE_CURVE_WITH_KNOTS('',3,(#6006,#6007,#6008,#6009,#6010,#6011),
 .UNSPECIFIED.,.F.,.F.,(4,1,1,4),(32.9594405895371,33.358149694947,34.3563443992555,
34.5575191894877),.UNSPECIFIED.);
#1153=B_SPLINE_CURVE_WITH_KNOTS('',3,(#6013,#6014,#6015,#6016,#6017),
 .UNSPECIFIED.,.F.,.F.,(4,1,4),(32.9608271762519,33.6713022573751,34.5575102647709),
 .UNSPECIFIED.);
#1154=B_SPLINE_CURVE_WITH_KNOTS('',3,(#6018,#6019,#6020,#6021,#6022,#6023,
#6024,#6025,#6026,#6027,#6028,#6029,#6030,#6031,#6032,#6033,#6034,#6035,
#6036,#6037,#6038,#6039,#6040,#6041,#6042,#6043,#6044,#6045,#6046,#6047,
#6048,#6049,#6050,#6051,#6052,#6053,#6054,#6055,#6056,#6057,#6058,#6059,
#6060,#6061,#6062,#6063,#6064,#6065,#6066,#6067,#6068,#6069,#6070,#6071,
#6072,#6073,#6074,#6075,#6076,#6077,#6078,#6079,#6080,#6081,#6082,#6083,
#6084,#6085,#6086,#6087,#6088,#6089,#6090,#6091,#6092,#6093,#6094,#6095,
#6096,#6097,#6098,#6099,#6100,#6101,#6102,#6103,#6104,#6105,#6106,#6107,
#6108,#6109,#6110,#6111,#6112,#6113,#6114,#6115,#6116,#6117,#6118,#6119,
#6120,#6121,#6122,#6123,#6124,#6125,#6126,#6127,#6128,#6129,#6130,#6131,
#6132,#6133,#6134,#6135,#6136,#6137,#6138,#6139,#6140,#6141,#6142,#6143,
#6144,#6145,#6146,#6147,#6148,#6149,#6150,#6151,#6152,#6153,#6154,#6155,
#6156,#6157,#6158,#6159,#6160,#6161,#6162,#6163,#6164,#6165,#6166,#6167,
#6168,#6169),.UNSPECIFIED.,.F.,.F.,(4,2,2,2,2,2,2,2,2,2,2,2,2,2,2,2,2,2,
2,2,2,2,2,2,2,2,2,2,2,2,2,2,2,2,2,2,2,2,2,2,2,2,2,2,2,2,2,2,2,2,2,2,2,2,
2,2,2,2,2,2,2,2,2,2,2,2,2,2,2,2,2,2,2,2,2,4),(-2.23888494972284,-2.22991776855793,
-2.22447064320661,-2.22191829216988,-2.21989477343009,-2.21776847377992,
-2.21502874476971,-2.20893402279126,-2.18787843436243,-2.16966634347861,
-2.14385238080136,-2.13606038366673,-2.13171077947681,-2.12794768118234,
-2.12328524358438,-2.11390205737419,-2.07246864712722,-2.05027458125105,
-2.04489827929598,-2.04226229222838,-2.04035089005686,-2.03776646712269,
-2.0328105326407,-1.99791659798478,-1.96864883524523,-1.95927121403217,
-1.95460974539526,-1.95084658102242,-1.94649595728929,-1.93891035281729,
-1.89754680244139,-1.87904083706616,-1.86884897296706,-1.86549209633338,
-1.86327753791409,-1.86098243262719,-1.85724781425568,-1.84435404247657,
-1.80361547729748,-1.78470675362083,-1.77873969519656,-1.77476942506272,
-1.77092850577831,-1.76629564503759,-1.75480186338448,-1.71587013709037,
-1.69449471669221,-1.6892066322397,-1.68658769916922,-1.68467704547633,
-1.68207654389007,-1.67688276164301,-1.64448591367606,-1.63262573013931,
-1.61610562983729,-1.60466923401097,-1.59964695878773,-1.59584552599926,
-1.59170494698949,-1.5849177429812,-1.554669575998,-1.53244795233212,-1.51446840999572,
-1.51049555511708,-1.50814869586371,-1.50599106650872,-1.50332518743687,
-1.49656138600397,-1.45787430738769,-1.43249347062081,-1.42475990429867,
-1.42042205696215,-1.41665756715559,-1.4119784002815,-1.4046112824739,-1.40437359183403),
 .UNSPECIFIED.);
#1155=B_SPLINE_CURVE_WITH_KNOTS('',3,(#6175,#6176,#6177,#6178,#6179,#6180,
#6181,#6182,#6183,#6184,#6185,#6186,#6187,#6188,#6189,#6190,#6191,#6192,
#6193,#6194,#6195,#6196,#6197,#6198,#6199,#6200,#6201,#6202,#6203,#6204,
#6205,#6206,#6207,#6208,#6209,#6210,#6211,#6212,#6213,#6214,#6215,#6216,
#6217,#6218,#6219,#6220,#6221,#6222,#6223,#6224,#6225,#6226,#6227,#6228,
#6229,#6230,#6231,#6232,#6233,#6234,#6235,#6236,#6237,#6238,#6239,#6240,
#6241,#6242,#6243,#6244,#6245,#6246,#6247,#6248,#6249,#6250,#6251,#6252,
#6253,#6254,#6255,#6256,#6257,#6258,#6259,#6260,#6261,#6262,#6263,#6264,
#6265,#6266,#6267,#6268,#6269,#6270,#6271,#6272,#6273,#6274,#6275,#6276,
#6277,#6278,#6279,#6280,#6281,#6282,#6283,#6284,#6285,#6286,#6287,#6288,
#6289,#6290,#6291,#6292,#6293,#6294,#6295,#6296,#6297,#6298,#6299,#6300,
#6301,#6302,#6303,#6304,#6305,#6306,#6307,#6308,#6309,#6310,#6311,#6312,
#6313,#6314,#6315,#6316,#6317,#6318,#6319,#6320,#6321,#6322),
 .UNSPECIFIED.,.F.,.F.,(4,2,2,2,2,2,2,2,2,2,2,2,2,2,2,2,2,2,2,2,2,2,2,2,
2,2,2,2,2,2,2,2,2,2,2,2,2,2,2,2,2,2,2,2,2,2,2,2,2,2,2,2,2,2,2,2,2,2,2,2,
2,2,2,2,2,2,2,2,2,2,2,2,2,4),(-0.835099924428374,-0.810230319348001,-0.804896130565269,
-0.802268377014195,-0.800146299250092,-0.797444671956707,-0.791720718154825,
-0.783761495584802,-0.76005780011584,-0.726728468131525,-0.719363533194796,
-0.714685219878248,-0.71092110576457,-0.70658334156592,-0.69884901195783,
-0.673458960429975,-0.634756499650488,-0.627989293535211,-0.625322962005017,
-0.623165325271974,-0.620818865337488,-0.616847515854485,-0.59888758745142,
-0.576676092912076,-0.54644768251051,-0.539660204241827,-0.535519716308051,
-0.531718510580919,-0.526696749457739,-0.515262844600596,-0.498745486707646,
-0.487103824026872,-0.454413034292759,-0.449239542055546,-0.446643067818346,
-0.444732272546319,-0.442109216499667,-0.436799720433161,-0.415227032788622,
-0.375690485550125,-0.364600414407815,-0.359688848510703,-0.355891171960493,
-0.35173917187912,-0.344896737736136,-0.336636791651806,-0.318863385154281,
-0.284112077379857,-0.273620116100306,-0.270127168635037,-0.268106390492079,
-0.265898441440772,-0.262574397053666,-0.252664479586328,-0.234986866661226,
-0.19213003390502,-0.184740608673265,-0.180432716329455,-0.176701275542952,
-0.171998743506043,-0.16240040782514,-0.138024613707217,-0.10870919764151,
-0.0962332329690868,-0.0925351436016178,-0.0902480445649851,-0.0880276089129058,
-0.0846416658687451,-0.074190627067205,-0.0548973537364689,-0.0155466790190831,
-0.00753311737622712,-0.00341159348289976,-0.000525934153839705),
 .UNSPECIFIED.);
#1156=B_SPLINE_CURVE_WITH_KNOTS('',3,(#6323,#6324,#6325,#6326,#6327,#6328,
#6329,#6330,#6331,#6332,#6333,#6334,#6335,#6336,#6337,#6338,#6339,#6340,
#6341,#6342,#6343,#6344,#6345,#6346,#6347,#6348,#6349,#6350,#6351,#6352,
#6353,#6354,#6355,#6356,#6357,#6358,#6359,#6360,#6361,#6362,#6363,#6364,
#6365,#6366,#6367,#6368,#6369,#6370,#6371),.UNSPECIFIED.,.F.,.F.,(4,3,3,
3,3,3,3,3,3,3,3,3,3,3,3,3,4),(39.2426799043403,39.347317920798,39.4553587897862,
39.5666280192012,39.6743719212775,39.7820499685097,39.8897009618222,39.9973636575694,
40.1051459330372,40.2130005998416,40.3210371210927,40.3455126251065,40.4593059977434,
40.5727552393315,40.6859938246744,40.798974097679,40.8407044963078),
 .UNSPECIFIED.);
#1157=B_SPLINE_CURVE_WITH_KNOTS('',3,(#6372,#6373,#6374,#6375,#6376,#6377,
#6378,#6379,#6380,#6381,#6382,#6383,#6384,#6385,#6386,#6387,#6388,#6389,
#6390,#6391,#6392,#6393,#6394,#6395,#6396,#6397,#6398,#6399,#6400,#6401,
#6402,#6403,#6404,#6405,#6406,#6407,#6408,#6409,#6410,#6411,#6412,#6413,
#6414,#6415,#6416,#6417,#6418,#6419,#6420,#6421,#6422,#6423,#6424,#6425,
#6426,#6427,#6428,#6429,#6430,#6431,#6432,#6433,#6434,#6435,#6436,#6437,
#6438,#6439,#6440,#6441,#6442,#6443,#6444,#6445,#6446,#6447,#6448,#6449,
#6450,#6451,#6452,#6453,#6454,#6455,#6456,#6457,#6458,#6459,#6460,#6461,
#6462,#6463,#6464,#6465,#6466,#6467,#6468,#6469,#6470,#6471,#6472,#6473,
#6474,#6475,#6476,#6477,#6478,#6479,#6480,#6481,#6482,#6483,#6484,#6485,
#6486,#6487,#6488,#6489,#6490,#6491,#6492,#6493,#6494,#6495,#6496,#6497,
#6498,#6499,#6500,#6501,#6502,#6503,#6504,#6505,#6506,#6507,#6508,#6509,
#6510,#6511,#6512,#6513,#6514,#6515,#6516,#6517,#6518,#6519,#6520,#6521,
#6522,#6523,#6524,#6525,#6526,#6527,#6528,#6529,#6530,#6531,#6532,#6533,
#6534,#6535,#6536,#6537,#6538,#6539,#6540,#6541,#6542,#6543,#6544,#6545,
#6546,#6547,#6548,#6549,#6550,#6551,#6552,#6553,#6554,#6555,#6556,#6557),
 .UNSPECIFIED.,.F.,.F.,(4,2,2,2,2,2,2,2,2,2,2,2,2,2,2,2,2,2,2,2,2,2,2,2,
2,2,2,2,2,2,2,2,2,2,2,2,2,2,2,2,2,2,2,2,2,2,2,2,2,2,2,2,2,2,2,2,2,2,2,2,
2,2,2,2,2,2,2,2,2,2,2,2,2,2,2,2,2,2,2,2,2,2,2,2,2,2,2,2,2,2,2,2,4),(-1.40437359183403,
-1.37123442544774,-1.34752963779357,-1.33956894550668,-1.33384453706723,
-1.33114265739486,-1.32902037709875,-1.32639236697421,-1.32105767193388,
-1.28990184687834,-1.27710833130175,-1.26053819930053,-1.24907775154556,
-1.24405147443566,-1.24024940402294,-1.23611045005564,-1.22933132030553,
-1.1991424444891,-1.17718888992443,-1.16481053221377,-1.15695984650571,
-1.15390650964041,-1.15174763436364,-1.14934515565329,-1.14511413330171,
-1.1199654897537,-1.07619341358872,-1.06892966170554,-1.06464923613406,
-1.0612555821067,-1.05667875748375,-1.04774607909163,-1.0360187374714,-1.00243054455778,
-0.981420876710011,-0.977242959541184,-0.974851927051027,-0.972688952611354,
-0.969609890907095,-0.96158130833031,-0.948791070416998,-0.911037219829708,
-0.895295885708175,-0.889507924932764,-0.88596636520286,-0.882113005965861,
-0.876761106568744,-0.863143851728035,-0.841650542388842,-0.80749697430888,
-0.800992055473671,-0.798368262274408,-0.796220606248343,-0.793852062063708,
-0.789778743192625,-0.769603171631479,-0.724976386629526,-0.714953988896045,
-0.710174271931691,-0.706401887754161,-0.702133000275573,-0.694731715330455,
-0.662688812809577,-0.627098897825888,-0.622213482154788,-0.619643997664196,
-0.617538915753009,-0.614779745974369,-0.608740756103967,-0.600182111874869,
-0.572873372681339,-0.544179070275189,-0.536835062276827,-0.532162650611676,
-0.528398714254533,-0.524056114345843,-0.5162990981695,-0.490744904305246,
-0.451146436953167,-0.445598441642736,-0.44288337641325,-0.44071350468291,
-0.438389667197007,-0.434523083461308,-0.418400108311522,-0.366386013304921,
-0.358997698073502,-0.354312637345431,-0.350548095703286,-0.346215342549465,
-0.338505260339425,-0.310188566919195,-0.285073042962578),.UNSPECIFIED.);
#1158=B_SPLINE_CURVE_WITH_KNOTS('',3,(#6562,#6563,#6564,#6565,#6566,#6567,
#6568,#6569,#6570,#6571,#6572,#6573,#6574,#6575,#6576,#6577,#6578,#6579,
#6580,#6581,#6582,#6583,#6584,#6585,#6586,#6587,#6588,#6589,#6590,#6591,
#6592,#6593,#6594,#6595,#6596,#6597,#6598,#6599,#6600,#6601,#6602,#6603,
#6604,#6605,#6606,#6607,#6608,#6609,#6610,#6611,#6612,#6613,#6614,#6615,
#6616,#6617,#6618,#6619,#6620,#6621,#6622,#6623,#6624,#6625,#6626,#6627,
#6628,#6629,#6630,#6631,#6632,#6633,#6634,#6635,#6636,#6637,#6638,#6639,
#6640,#6641,#6642,#6643,#6644,#6645,#6646,#6647,#6648,#6649,#6650,#6651,
#6652,#6653,#6654,#6655,#6656,#6657,#6658,#6659,#6660,#6661,#6662,#6663,
#6664,#6665,#6666,#6667,#6668,#6669,#6670,#6671,#6672,#6673,#6674,#6675,
#6676,#6677,#6678,#6679,#6680,#6681,#6682,#6683,#6684,#6685,#6686,#6687,
#6688,#6689,#6690,#6691,#6692,#6693,#6694,#6695,#6696,#6697,#6698,#6699,
#6700,#6701,#6702,#6703,#6704,#6705,#6706,#6707,#6708,#6709,#6710,#6711,
#6712,#6713,#6714,#6715,#6716,#6717,#6718,#6719,#6720,#6721,#6722,#6723,
#6724,#6725,#6726,#6727,#6728,#6729,#6730,#6731,#6732,#6733,#6734,#6735,
#6736,#6737,#6738,#6739,#6740,#6741,#6742,#6743,#6744,#6745,#6746,#6747,
#6748,#6749,#6750,#6751),.UNSPECIFIED.,.F.,.F.,(4,2,2,2,2,2,2,2,2,2,2,2,
2,2,2,2,2,2,2,2,2,2,2,2,2,2,2,2,2,2,2,2,2,2,2,2,2,2,2,2,2,2,2,2,2,2,2,2,
2,2,2,2,2,2,2,2,2,2,2,2,2,2,2,2,2,2,2,2,2,2,2,2,2,2,2,2,2,2,2,2,2,2,2,2,
2,2,2,2,2,2,2,2,2,2,4),(-1.95419705041876,-1.95099509657436,-1.94335603423285,
-1.89991425942924,-1.87506559070961,-1.87085029414465,-1.86845141700778,
-1.86629169624077,-1.86323154906988,-1.85589494163826,-1.80915527702303,
-1.78941037574571,-1.78336666657204,-1.77938126023139,-1.77555177097439,
-1.77011478780303,-1.75687520202681,-1.71971687152613,-1.69894795789413,
-1.69372753446967,-1.69112204521488,-1.68899928354412,-1.6862729303428,
-1.68061920244923,-1.64560251554659,-1.62383557245409,-1.61010952998578,
-1.60474301590359,-1.60088747043224,-1.59734954579938,-1.59158053314671,
-1.57599794538798,-1.53805844930273,-1.5252395640355,-1.51719964584465,
-1.51411912755031,-1.51195609974106,-1.50956606370411,-1.50539209599044,
-1.48448455657626,-1.45085051616374,-1.43911885055448,-1.43018312798703,
-1.42560600193481,-1.42221257001728,-1.41793303258227,-1.41067227172661,
-1.36685718427406,-1.34377191808452,-1.33830282624568,-1.33564914858626,
-1.33352753047315,-1.3308533889611,-1.32527638798234,-1.28500681146791,
-1.25934693277238,-1.25157594831113,-1.24723074868244,-1.24346741272986,
-1.23879943896024,-1.2314698664428,-1.1962869213581,-1.17389058740369,-1.16617028239694,
-1.16057494815006,-1.15789737507523,-1.15577576095328,-1.15312549402477,
-1.14767412692595,-1.11976092188052,-1.08198674324006,-1.07476016775468,
-1.07012217598063,-1.06636070172582,-1.06199273348142,-1.05411036107367,
-1.02761652170471,-1.00975943176876,-0.986126109116485,-0.981905770012072,
-0.979505779977728,-0.977346392827614,-0.974288562634894,-0.966405257133201,
-0.953952236184314,-0.930399287942635,-0.901801161853786,-0.89511851665121,
-0.891000170280617,-0.887191963350469,-0.882119951237423,-0.870373676231296,
-0.853196610132522,-0.841453580091553,-0.835099924428374),.UNSPECIFIED.);
#1159=B_SPLINE_CURVE_WITH_KNOTS('',3,(#6753,#6754,#6755,#6756,#6757,#6758,
#6759,#6760,#6761,#6762,#6763,#6764,#6765,#6766,#6767,#6768,#6769,#6770,
#6771,#6772,#6773,#6774,#6775,#6776,#6777,#6778,#6779,#6780,#6781,#6782,
#6783,#6784,#6785,#6786,#6787,#6788,#6789,#6790,#6791,#6792,#6793,#6794,
#6795,#6796,#6797,#6798,#6799,#6800,#6801,#6802,#6803,#6804,#6805,#6806,
#6807,#6808),.UNSPECIFIED.,.F.,.F.,(4,2,2,2,2,2,2,2,2,2,2,2,2,2,2,2,2,2,
2,2,2,2,2,2,2,2,2,4),(-0.285073042962578,-0.279553666108781,-0.268860677228453,
-0.265344191924806,-0.263318928126342,-0.261115262971523,-0.257812524684666,
-0.248081258600964,-0.230913628765321,-0.187069317157601,-0.179816393831322,
-0.175538464730903,-0.172144677675042,-0.167564926100631,-0.1586163724922,
-0.1468608393431,-0.113089336365138,-0.0923072130143463,-0.0881367138826751,
-0.0857473423440587,-0.0835838714087559,-0.0805013269290881,-0.072447874665844,
-0.0595990213919607,-0.0169573151041265,-0.00623282049412229,-0.002812104231931,
-0.000526075114705878),.UNSPECIFIED.);
#1160=B_SPLINE_CURVE_WITH_KNOTS('',3,(#6809,#6810,#6811,#6812,#6813,#6814,
#6815,#6816,#6817,#6818,#6819,#6820,#6821,#6822,#6823,#6824,#6825,#6826,
#6827,#6828,#6829,#6830,#6831,#6832,#6833,#6834,#6835,#6836,#6837,#6838,
#6839,#6840,#6841,#6842,#6843,#6844,#6845,#6846,#6847,#6848,#6849,#6850,
#6851,#6852,#6853,#6854,#6855,#6856,#6857,#6858,#6859,#6860,#6861,#6862,
#6863,#6864,#6865,#6866,#6867,#6868,#6869,#6870,#6871,#6872,#6873,#6874,
#6875,#6876,#6877,#6878,#6879,#6880,#6881,#6882,#6883,#6884,#6885,#6886,
#6887,#6888,#6889,#6890,#6891,#6892,#6893,#6894,#6895,#6896,#6897,#6898,
#6899,#6900,#6901,#6902,#6903,#6904,#6905,#6906,#6907,#6908,#6909,#6910,
#6911,#6912,#6913,#6914,#6915,#6916,#6917,#6918,#6919,#6920,#6921,#6922,
#6923,#6924,#6925,#6926,#6927,#6928,#6929,#6930,#6931,#6932,#6933,#6934,
#6935,#6936,#6937,#6938,#6939,#6940,#6941,#6942,#6943,#6944,#6945,#6946,
#6947,#6948,#6949,#6950,#6951,#6952,#6953,#6954,#6955,#6956),
 .UNSPECIFIED.,.F.,.F.,(4,2,2,2,2,2,2,2,2,2,2,2,2,2,2,2,2,2,2,2,2,2,2,2,
2,2,2,2,2,2,2,2,2,2,2,2,2,2,2,2,2,2,2,2,2,2,2,2,2,2,2,2,2,2,2,2,2,2,2,2,
2,2,2,2,2,2,2,2,2,2,2,2,2,4),(-2.23857561374812,-2.23666385583856,-2.2340934120843,
-2.23009258721063,-2.22419325848768,-2.20619608151607,-2.19090605687411,
-2.17043683124224,-2.15225191817315,-2.14826971816482,-2.14592139942912,
-2.14376573100267,-2.14110559550224,-2.13449203871347,-2.09568856819996,
-2.07029326499371,-2.06255934505371,-2.05822247095775,-2.05445947610837,
-2.04978301278047,-2.04242188441953,-2.00865447681867,-1.98525790756218,
-1.97735400463938,-1.97166046700269,-1.96896494610926,-1.96684359883701,
-1.96421168899267,-1.95885368261893,-1.92912983707482,-1.89155161913244,
-1.88436917889393,-1.8801467846608,-1.87636772192449,-1.87151344137471,
-1.86352917809948,-1.81252018407983,-1.79646904009444,-1.7926075584725,
-1.79028526412203,-1.78811549736986,-1.78539927151285,-1.77844064281174,
-1.74003635299827,-1.71471290957797,-1.70698834410922,-1.70265308793857,
-1.69888948105043,-1.6942096348079,-1.68683780154111,-1.65393798808469,
-1.62989527272789,-1.62187564888924,-1.61612027753882,-1.6134131074963,
-1.61129123618027,-1.60866939319371,-1.60336428715806,-1.57241511393776,
-1.54749150698952,-1.53258949837975,-1.52706691580707,-1.52318358899077,
-1.51967589277267,-1.51497195103688,-1.50319238607423,-1.46462085528223,
-1.44336862512482,-1.43809465985453,-1.43547879772472,-1.43356863123409,
-1.43096621393663,-1.42576103694743,-1.40411156028844),.UNSPECIFIED.);
#1161=B_SPLINE_CURVE_WITH_KNOTS('',3,(#6962,#6963,#6964,#6965,#6966,#6967,
#6968,#6969,#6970,#6971,#6972,#6973,#6974,#6975,#6976,#6977,#6978,#6979,
#6980,#6981,#6982,#6983,#6984,#6985,#6986,#6987,#6988,#6989,#6990,#6991,
#6992,#6993,#6994,#6995,#6996,#6997,#6998,#6999,#7000,#7001,#7002,#7003,
#7004,#7005,#7006,#7007,#7008,#7009,#7010,#7011,#7012,#7013,#7014,#7015,
#7016,#7017,#7018,#7019,#7020,#7021,#7022,#7023,#7024,#7025,#7026,#7027,
#7028,#7029,#7030,#7031,#7032,#7033,#7034,#7035,#7036,#7037,#7038,#7039,
#7040,#7041,#7042,#7043,#7044,#7045,#7046,#7047,#7048,#7049,#7050,#7051,
#7052,#7053,#7054,#7055,#7056,#7057,#7058,#7059,#7060,#7061,#7062,#7063,
#7064,#7065,#7066,#7067,#7068,#7069,#7070,#7071,#7072,#7073,#7074,#7075,
#7076,#7077,#7078,#7079,#7080,#7081,#7082,#7083,#7084,#7085,#7086,#7087,
#7088,#7089,#7090,#7091,#7092,#7093,#7094,#7095,#7096,#7097),
 .UNSPECIFIED.,.F.,.F.,(4,2,2,2,2,2,2,2,2,2,2,2,2,2,2,2,2,2,2,2,2,2,2,2,
2,2,2,2,2,2,2,2,2,2,2,2,2,2,2,2,2,2,2,2,2,2,2,2,2,2,2,2,2,2,2,2,2,2,2,2,
2,2,2,2,2,2,2,4),(-0.83510473565426,-0.807059091250157,-0.794248944238828,
-0.788888281898605,-0.785072276945066,-0.781065979555653,-0.774919202696639,
-0.753969699442934,-0.731087482698737,-0.705729883148012,-0.700270175960026,
-0.697618575084768,-0.69549732017242,-0.692822002462581,-0.687237232275534,
-0.679536961050213,-0.657240309233987,-0.621967947033965,-0.614643791100851,
-0.609977772140206,-0.606215108268336,-0.601869681911633,-0.594095560427073,
-0.568407118507129,-0.527431822374366,-0.522306693016003,-0.519720011857097,
-0.517809058982425,-0.515176404745292,-0.509816001002867,-0.487766096186353,
-0.446763188010461,-0.437032466896656,-0.43230609171582,-0.428538863753342,
-0.424236117433176,-0.41666977793013,-0.385854931560725,-0.351305194221669,
-0.345096691777328,-0.34233722111936,-0.340209517527547,-0.337667515641714,
-0.332765712758342,-0.303531750266518,-0.266259382527087,-0.259006079374804,
-0.254360551254719,-0.250598995790071,-0.246237674293427,-0.238386499891509,
-0.212124957649786,-0.172168692303313,-0.166846565800831,-0.164221259453316,
-0.162099263379596,-0.15939533519259,-0.153658354972325,-0.145674488158747,
-0.121830870754642,-0.0886967464382455,-0.0813294240915939,-0.0766505948237803,
-0.0728866835996491,-0.0685498339497959,-0.0608190313853347,-0.0354526272559785,
-0.000526495403762602),.UNSPECIFIED.);
#1162=B_SPLINE_CURVE_WITH_KNOTS('',3,(#7098,#7099,#7100,#7101,#7102,#7103,
#7104,#7105,#7106,#7107,#7108,#7109,#7110,#7111,#7112,#7113,#7114,#7115,
#7116,#7117,#7118,#7119,#7120,#7121,#7122,#7123,#7124,#7125,#7126,#7127,
#7128,#7129,#7130,#7131,#7132,#7133,#7134,#7135,#7136,#7137,#7138,#7139,
#7140,#7141,#7142,#7143,#7144,#7145,#7146,#7147,#7148,#7149,#7150,#7151,
#7152,#7153),.UNSPECIFIED.,.F.,.F.,(4,2,2,2,2,2,2,2,2,2,2,2,2,2,2,2,2,2,
2,2,2,2,2,2,2,2,2,4),(-2.23859886574399,-2.23016997570174,-2.22724347696598,
-2.22509778038061,-2.22304729674188,-2.22064081803864,-2.21638940119625,
-2.19887690410067,-2.16438742506128,-2.1449527001157,-2.13893733858008,
-2.13495785335683,-2.13112475931472,-2.12652164794244,-2.11536814953201,
-2.07614378249324,-2.05467230085902,-2.04937433483211,-2.0467537992826,
-2.04484343810543,-2.04224546994443,-2.03722372250726,-2.00306363251165,
-1.97305660076362,-1.96376339585746,-1.95911833261462,-1.95535679587401,
-1.95419705041876),.UNSPECIFIED.);
#1163=B_SPLINE_CURVE_WITH_KNOTS('',3,(#7154,#7155,#7156,#7157,#7158,#7159,
#7160,#7161,#7162,#7163,#7164,#7165,#7166,#7167,#7168,#7169,#7170,#7171,
#7172,#7173,#7174,#7175,#7176,#7177,#7178,#7179,#7180,#7181,#7182,#7183,
#7184,#7185,#7186,#7187,#7188,#7189,#7190,#7191,#7192,#7193,#7194,#7195,
#7196,#7197,#7198,#7199,#7200,#7201,#7202,#7203,#7204,#7205,#7206,#7207,
#7208,#7209,#7210,#7211,#7212,#7213,#7214,#7215,#7216,#7217,#7218,#7219,
#7220,#7221,#7222,#7223,#7224,#7225,#7226,#7227,#7228,#7229,#7230,#7231,
#7232,#7233,#7234,#7235,#7236,#7237,#7238,#7239,#7240,#7241,#7242,#7243,
#7244,#7245,#7246,#7247,#7248,#7249,#7250,#7251,#7252,#7253,#7254,#7255,
#7256,#7257,#7258,#7259,#7260,#7261,#7262,#7263,#7264,#7265,#7266,#7267,
#7268,#7269,#7270,#7271,#7272,#7273,#7274,#7275,#7276,#7277,#7278,#7279,
#7280,#7281,#7282,#7283,#7284,#7285,#7286,#7287,#7288,#7289,#7290,#7291,
#7292,#7293,#7294,#7295,#7296,#7297,#7298,#7299,#7300,#7301,#7302,#7303,
#7304,#7305,#7306,#7307,#7308,#7309,#7310,#7311,#7312,#7313,#7314,#7315,
#7316,#7317,#7318,#7319,#7320,#7321,#7322,#7323,#7324,#7325,#7326,#7327,
#7328,#7329,#7330,#7331,#7332,#7333,#7334,#7335,#7336,#7337,#7338,#7339,
#7340,#7341,#7342,#7343),.UNSPECIFIED.,.F.,.F.,(4,2,2,2,2,2,2,2,2,2,2,2,
2,2,2,2,2,2,2,2,2,2,2,2,2,2,2,2,2,2,2,2,2,2,2,2,2,2,2,2,2,2,2,2,2,2,2,2,
2,2,2,2,2,2,2,2,2,2,2,2,2,2,2,2,2,2,2,2,2,2,2,2,2,2,2,2,2,2,2,2,2,2,2,2,
2,2,2,2,2,2,2,2,2,2,4),(-1.40411156028844,-1.39349542557748,-1.36935987545478,
-1.35473797928305,-1.34925131297417,-1.34537445729729,-1.34186020981609,
-1.33712872630781,-1.32517580104704,-1.28678083561332,-1.27108739193897,
-1.26481221899932,-1.26002549128862,-1.25750686692788,-1.25537609341367,
-1.25258406971052,-1.24618619485546,-1.20692794327319,-1.18144655746937,
-1.17370009162669,-1.16936012333648,-1.16559662849119,-1.16092238061841,
-1.15357054764298,-1.11942673560362,-1.08784664187256,-1.08254616461267,
-1.07992503533727,-1.07780287823297,-1.07509426121558,-1.0693320686284,
-1.06130086376561,-1.03718984474042,-1.00441413216787,-0.997041813059222,
-0.992361495680813,-0.988597433613231,-0.984261566797749,-0.976535753034919,
-0.951206572032963,-0.912829974784523,-0.905819434608511,-0.903095179753961,
-0.900923137884646,-0.898603804428527,-0.894757087456774,-0.878940018869739,
-0.83075013623136,-0.819907281922897,-0.815037208524472,-0.811245612843338,
-0.807073897687486,-0.800135930020867,-0.764276356933327,-0.732100216115735,
-0.726880331832764,-0.724274918542289,-0.722364713349845,-0.719751555505083,
-0.714492055170275,-0.693372844261857,-0.655183432209298,-0.64304735200466,
-0.638290363807922,-0.634769988408522,-0.630898851688508,-0.625444407383234,
-0.611070142823161,-0.587610459950588,-0.554188019843694,-0.549050425734941,
-0.546461192345198,-0.544550262122613,-0.541920076882484,-0.536572921944452,
-0.514648747427636,-0.474039109303757,-0.464077047169949,-0.4592416762617,
-0.455463939474107,-0.451229172488678,-0.443990541578409,-0.435104383296082,
-0.415083011447363,-0.384841681837122,-0.373635655274898,-0.370061264147062,
-0.367801128323677,-0.365558213430779,-0.362064012666355,-0.350585761782471,
-0.327888579904079,-0.293170013073975,-0.285831970878823,-0.285021347106446),
 .UNSPECIFIED.);
#1164=B_SPLINE_CURVE_WITH_KNOTS('',3,(#7348,#7349,#7350,#7351,#7352,#7353,
#7354,#7355,#7356,#7357,#7358,#7359,#7360,#7361,#7362,#7363,#7364,#7365,
#7366,#7367,#7368,#7369,#7370,#7371,#7372,#7373,#7374,#7375,#7376,#7377,
#7378,#7379,#7380,#7381,#7382,#7383,#7384,#7385,#7386,#7387,#7388,#7389,
#7390,#7391,#7392,#7393,#7394,#7395,#7396,#7397,#7398,#7399,#7400,#7401,
#7402,#7403,#7404,#7405,#7406,#7407,#7408,#7409,#7410,#7411,#7412,#7413,
#7414,#7415,#7416,#7417,#7418,#7419,#7420,#7421,#7422,#7423,#7424,#7425,
#7426,#7427,#7428,#7429,#7430,#7431,#7432,#7433,#7434,#7435,#7436,#7437,
#7438,#7439,#7440,#7441,#7442,#7443,#7444,#7445,#7446,#7447,#7448,#7449,
#7450,#7451,#7452,#7453,#7454,#7455,#7456,#7457,#7458,#7459,#7460,#7461,
#7462,#7463,#7464,#7465,#7466,#7467,#7468,#7469,#7470,#7471,#7472,#7473,
#7474,#7475,#7476,#7477,#7478,#7479,#7480,#7481,#7482,#7483,#7484,#7485,
#7486,#7487,#7488,#7489,#7490,#7491,#7492,#7493,#7494,#7495,#7496,#7497,
#7498,#7499,#7500,#7501,#7502,#7503,#7504,#7505,#7506,#7507,#7508,#7509,
#7510,#7511,#7512,#7513,#7514,#7515,#7516,#7517,#7518,#7519,#7520,#7521,
#7522,#7523,#7524,#7525,#7526,#7527,#7528,#7529,#7530,#7531,#7532,#7533,
#7534,#7535,#7536,#7537,#7538,#7539,#7540,#7541,#7542,#7543,#7544,#7545,
#7546,#7547),.UNSPECIFIED.,.F.,.F.,(4,2,2,2,2,2,2,2,2,2,2,2,2,2,2,2,2,2,
2,2,2,2,2,2,2,2,2,2,2,2,2,2,2,2,2,2,2,2,2,2,2,2,2,2,2,2,2,2,2,2,2,2,2,2,
2,2,2,2,2,2,2,2,2,2,2,2,2,2,2,2,2,2,2,2,2,2,2,2,2,2,2,2,2,2,2,2,2,2,2,2,
2,2,2,2,2,2,2,2,2,4),(-1.95389506130437,-1.94961407086964,-1.94435265691815,
-1.9417394763262,-1.93982967560218,-1.93722540144905,-1.93217238412767,
-1.89841999475128,-1.88910996699134,-1.87181659205363,-1.86001599820056,
-1.85493622470532,-1.8511276740487,-1.84701417635579,-1.84035134606648,
-1.81268413208584,-1.78850716862925,-1.77582103745545,-1.76783848349445,
-1.76476668612379,-1.76260547966791,-1.76021256979286,-1.75602354976164,
-1.73457015197743,-1.70139011953736,-1.68973132370297,-1.68083751565559,
-1.67626915432287,-1.67287722664734,-1.66859303510394,-1.66130810579235,
-1.61768751473044,-1.6003961500096,-1.59062264733991,-1.5873153830201,-1.58511126646256,
-1.58308774125901,-1.57957835825508,-1.5689401084213,-1.53829815592585,
-1.50969215678852,-1.50214984669414,-1.49785244116081,-1.49408511785598,
-1.48935228332671,-1.47958438212244,-1.43860450025514,-1.4165581110702,
-1.41119840668634,-1.4085660720675,-1.40665535200453,-1.40406895956547,
-1.39894437893211,-1.35800115287627,-1.33232428381637,-1.32455198038943,
-1.32020713893897,-1.31644471811796,-1.31177866222187,-1.30445369728431,
-1.26915912477824,-1.24685262501099,-1.23915004915792,-1.23356460720518,
-1.23088926696933,-1.22876815160177,-1.22611691801824,-1.22065857037651,
-1.19528125124984,-1.17267928575953,-1.15154607074122,-1.14538494328039,
-1.14137584354151,-1.13756178738194,-1.13221168315488,-1.11948299799636,
-1.0995854202924,-1.0696506914718,-1.05804258353884,-1.05442601881422,-1.05215697126489,
-1.04992271780096,-1.04646843229878,-1.03537755616004,-1.01401815355054,
-0.977397958580947,-0.970116091790745,-0.965462467500581,-0.961700727744027,
-0.957346288875495,-0.949527612400665,-0.923506871345019,-0.883134127625715,
-0.87789155775808,-0.875281862505312,-0.873372002991157,-0.870763717472937,
-0.865528363713152,-0.84462382045794,-0.83510473565426),.UNSPECIFIED.);
#1165=B_SPLINE_CURVE_WITH_KNOTS('',3,(#7549,#7550,#7551,#7552,#7553,#7554,
#7555,#7556,#7557,#7558,#7559,#7560,#7561,#7562,#7563,#7564,#7565,#7566,
#7567,#7568,#7569,#7570,#7571,#7572,#7573,#7574,#7575,#7576,#7577,#7578,
#7579,#7580,#7581,#7582,#7583,#7584,#7585,#7586,#7587,#7588,#7589,#7590,
#7591,#7592,#7593,#7594,#7595,#7596,#7597,#7598,#7599,#7600,#7601,#7602,
#7603,#7604),.UNSPECIFIED.,.F.,.F.,(4,2,2,2,2,2,2,2,2,2,2,2,2,2,2,2,2,2,
2,2,2,2,2,2,2,2,2,4),(-0.285021347106446,-0.281161663193334,-0.277398373222973,
-0.273055360378498,-0.26529436340703,-0.239706237843135,-0.199900284683521,
-0.193933541577183,-0.191187489861275,-0.189063723903572,-0.186474581453647,
-0.181337663102854,-0.161304723832711,-0.115050076035869,-0.107866320922798,
-0.103240961868744,-0.0994803599945839,-0.0951028654889191,-0.0871730377536201,
-0.0603159778932275,-0.0331866955665843,-0.018623391917416,-0.0147530662472885,
-0.0124287244048125,-0.0104203730523619,-0.00822868690897723,-0.00481396187852919,
-0.000525490636961181),.UNSPECIFIED.);
#1166=B_SPLINE_CURVE_WITH_KNOTS('',3,(#7605,#7606,#7607,#7608,#7609,#7610,
#7611,#7612,#7613,#7614,#7615,#7616,#7617,#7618,#7619,#7620,#7621,#7622,
#7623,#7624,#7625,#7626,#7627,#7628,#7629,#7630,#7631,#7632,#7633,#7634,
#7635,#7636,#7637,#7638,#7639,#7640,#7641,#7642,#7643,#7644,#7645,#7646,
#7647,#7648,#7649,#7650,#7651,#7652,#7653,#7654,#7655,#7656,#7657,#7658,
#7659,#7660,#7661,#7662,#7663,#7664,#7665,#7666,#7667,#7668,#7669,#7670,
#7671,#7672,#7673,#7674,#7675,#7676,#7677,#7678,#7679,#7680,#7681,#7682,
#7683,#7684,#7685,#7686,#7687,#7688,#7689,#7690,#7691,#7692,#7693,#7694,
#7695,#7696,#7697,#7698,#7699,#7700,#7701,#7702,#7703,#7704,#7705,#7706,
#7707,#7708,#7709,#7710,#7711,#7712,#7713,#7714,#7715,#7716,#7717,#7718,
#7719,#7720,#7721,#7722,#7723,#7724,#7725,#7726,#7727,#7728,#7729,#7730,
#7731,#7732,#7733,#7734,#7735,#7736,#7737,#7738,#7739,#7740,#7741,#7742,
#7743,#7744),.UNSPECIFIED.,.F.,.F.,(4,2,2,2,2,2,2,2,2,2,2,2,2,2,2,2,2,2,
2,2,2,2,2,2,2,2,2,2,2,2,2,2,2,2,2,2,2,2,2,2,2,2,2,2,2,2,2,2,2,2,2,2,2,2,
2,2,2,2,2,2,2,2,2,2,2,2,2,2,2,4),(-2.23873337236619,-2.20260153586138,-2.18290354736451,
-2.17410529702119,-2.16692151586359,-2.16269877503993,-2.15891966849369,
-2.15406570341143,-2.14361974126213,-2.10338553776005,-2.08158050601579,
-2.07624669828436,-2.07361939563287,-2.07170894832296,-2.0691179794163,
-2.06397009729765,-2.03082745801115,-2.00722841399602,-1.99280304483619,
-1.98734252780382,-1.98347075456529,-1.97995221815648,-1.97520141296699,
-1.96311026933505,-1.92485882536148,-1.90920460026644,-1.90293934496288,
-1.89815850660555,-1.89564126320214,-1.89351057571928,-1.89071729755099,
-1.88431088936225,-1.84997724502122,-1.81924544384307,-1.81169873693335,
-1.80740023942076,-1.80363277032895,-1.79890083745404,-1.78913895509525,
-1.7481469466383,-1.72609562974091,-1.72073516954654,-1.71810258222976,
-1.71619173394012,-1.71360526029047,-1.70848079994277,-1.66753023018797,
-1.64185225415164,-1.63407947481888,-1.62973435244094,-1.62597168549879,
-1.62130532605614,-1.61397990297146,-1.5786737489019,-1.55637030653304,
-1.54866800941179,-1.54308260875925,-1.54040716761905,-1.53828591523418,
-1.53563445127925,-1.53017546094156,-1.50476967412082,-1.48213862790443,
-1.46805288800406,-1.45783577156451,-1.45302172687808,-1.44924644613653,
-1.44499963097781,-1.437702390342,-1.40420841399148),.UNSPECIFIED.);
#1167=B_SPLINE_CURVE_WITH_KNOTS('',3,(#7750,#7751,#7752,#7753,#7754,#7755,
#7756,#7757,#7758,#7759,#7760,#7761,#7762,#7763,#7764,#7765,#7766,#7767,
#7768,#7769,#7770,#7771,#7772,#7773,#7774,#7775,#7776,#7777,#7778,#7779,
#7780,#7781,#7782,#7783,#7784,#7785,#7786,#7787,#7788,#7789,#7790,#7791,
#7792,#7793,#7794,#7795,#7796,#7797,#7798,#7799,#7800,#7801,#7802,#7803,
#7804,#7805,#7806,#7807,#7808,#7809,#7810,#7811,#7812,#7813,#7814,#7815,
#7816,#7817,#7818,#7819,#7820,#7821,#7822,#7823,#7824,#7825,#7826,#7827,
#7828,#7829,#7830,#7831,#7832,#7833,#7834,#7835,#7836,#7837,#7838,#7839,
#7840,#7841,#7842,#7843,#7844,#7845,#7846,#7847,#7848,#7849,#7850,#7851,
#7852,#7853,#7854,#7855,#7856,#7857,#7858,#7859,#7860,#7861,#7862,#7863,
#7864,#7865,#7866,#7867,#7868,#7869,#7870,#7871,#7872,#7873,#7874,#7875,
#7876,#7877,#7878,#7879,#7880,#7881,#7882,#7883,#7884,#7885,#7886,#7887,
#7888,#7889,#7890,#7891),.UNSPECIFIED.,.F.,.F.,(4,2,2,2,2,2,2,2,2,2,2,2,
2,2,2,2,2,2,2,2,2,2,2,2,2,2,2,2,2,2,2,2,2,2,2,2,2,2,2,2,2,2,2,2,2,2,2,2,
2,2,2,2,2,2,2,2,2,2,2,2,2,2,2,2,2,2,2,2,2,2,4),(-0.834941232871745,-0.819338014613434,
-0.780419456840186,-0.773876897628689,-0.771228350000444,-0.769075182262562,
-0.76672028489106,-0.762709008813453,-0.743935227528527,-0.719696160537062,
-0.692151444314202,-0.685491273255296,-0.681377889244008,-0.677568419768757,
-0.672485879720932,-0.660671654104035,-0.643348347957285,-0.634390608508764,
-0.600233948948421,-0.595207024521789,-0.592607904272523,-0.590697485827355,
-0.588077895921618,-0.582785190975061,-0.561363093112121,-0.522274883487837,
-0.511014445225283,-0.506393652155711,-0.502556064184696,-0.49858242784488,
-0.492596844588132,-0.473488659060427,-0.431526252182873,-0.41984652524168,
-0.416222493416279,-0.413951549150567,-0.411718154216969,-0.408269305484565,
-0.397234586843687,-0.376066447351619,-0.339149533468926,-0.331878451887984,
-0.327227489186553,-0.323465256407915,-0.319107300980184,-0.311273966591775,
-0.285149694537114,-0.244944364750276,-0.239667356677667,-0.237050648384628,
-0.234928128784792,-0.23221401927413,-0.226422854751299,-0.218337265924506,
-0.193916179048666,-0.161693698825526,-0.154241741883327,-0.149538166080894,
-0.145772111928063,-0.14169416235255,-0.134597951492617,-0.125762832492979,
-0.105932740980304,-0.0761709353257024,-0.0643122292258017,-0.0606708060663044,
-0.0583959850014676,-0.056165596692382,-0.0527316363869023,-0.041839504113066,
-0.000526393493502488),.UNSPECIFIED.);
#1168=B_SPLINE_CURVE_WITH_KNOTS('',3,(#7892,#7893,#7894,#7895,#7896,#7897,
#7898,#7899,#7900,#7901,#7902,#7903,#7904,#7905,#7906,#7907,#7908,#7909,
#7910,#7911,#7912,#7913,#7914,#7915,#7916,#7917,#7918,#7919,#7920,#7921,
#7922,#7923,#7924,#7925,#7926,#7927,#7928,#7929,#7930,#7931,#7932,#7933,
#7934,#7935,#7936,#7937,#7938,#7939,#7940,#7941),.UNSPECIFIED.,.F.,.F.,
(4,2,2,2,2,2,2,2,2,2,2,2,2,2,2,2,2,2,2,2,2,2,2,2,4),(-2.23848733616259,
-2.22485318200342,-2.21633320517607,-2.21215613460426,-2.20862493584771,
-2.20485000070879,-2.20003279176477,-2.19217956066984,-2.16197540421594,
-2.12745580410469,-2.12212413723587,-2.11949737154508,-2.11758708314289,
-2.11499597865043,-2.10984679614268,-2.07674844291394,-2.05312696383485,
-2.03869388648012,-2.03323263556511,-2.02936094762936,-2.02584288805889,
-2.02109333083917,-2.00900968516074,-1.97075663324338,-1.95389506130437),
 .UNSPECIFIED.);
#1169=B_SPLINE_CURVE_WITH_KNOTS('',3,(#7942,#7943,#7944,#7945,#7946,#7947,
#7948,#7949,#7950,#7951,#7952,#7953,#7954,#7955,#7956,#7957,#7958,#7959,
#7960,#7961,#7962,#7963,#7964,#7965,#7966,#7967,#7968,#7969,#7970,#7971,
#7972,#7973,#7974,#7975,#7976,#7977,#7978,#7979,#7980,#7981,#7982,#7983,
#7984,#7985,#7986,#7987,#7988,#7989,#7990,#7991,#7992,#7993,#7994,#7995,
#7996,#7997,#7998,#7999,#8000,#8001,#8002,#8003,#8004,#8005,#8006,#8007,
#8008,#8009,#8010,#8011,#8012,#8013,#8014,#8015,#8016,#8017,#8018,#8019,
#8020,#8021,#8022,#8023,#8024,#8025,#8026,#8027,#8028,#8029,#8030,#8031,
#8032,#8033,#8034,#8035,#8036,#8037,#8038,#8039,#8040,#8041,#8042,#8043,
#8044,#8045,#8046,#8047,#8048,#8049,#8050,#8051,#8052,#8053,#8054,#8055,
#8056,#8057,#8058,#8059,#8060,#8061,#8062,#8063,#8064,#8065,#8066,#8067,
#8068,#8069,#8070,#8071,#8072,#8073,#8074,#8075,#8076,#8077,#8078,#8079,
#8080,#8081,#8082,#8083,#8084,#8085,#8086,#8087,#8088,#8089,#8090,#8091,
#8092,#8093,#8094,#8095,#8096,#8097,#8098,#8099,#8100,#8101,#8102,#8103,
#8104,#8105,#8106,#8107,#8108,#8109,#8110,#8111,#8112,#8113,#8114,#8115,
#8116,#8117,#8118,#8119,#8120,#8121,#8122,#8123,#8124,#8125,#8126,#8127,
#8128,#8129,#8130,#8131,#8132,#8133,#8134,#8135,#8136,#8137,#8138,#8139),
 .UNSPECIFIED.,.F.,.F.,(4,2,2,2,2,2,2,2,2,2,2,2,2,2,2,2,2,2,2,2,2,2,2,2,
2,2,2,2,2,2,2,2,2,2,2,2,2,2,2,2,2,2,2,2,2,2,2,2,2,2,2,2,2,2,2,2,2,2,2,2,
2,2,2,2,2,2,2,2,2,2,2,2,2,2,2,2,2,2,2,2,2,2,2,2,2,2,2,2,2,2,2,2,2,2,2,2,
2,2,4),(-1.40420841399148,-1.39355085824773,-1.37068095745477,-1.36523429056841,
-1.36258503480482,-1.36046356537884,-1.35778535404069,-1.3521859982408,
-1.31194709694592,-1.28629339955214,-1.27852358256444,-1.27417885925728,
-1.27041584373649,-1.26574815358256,-1.25841880912706,-1.22324735169539,
-1.20084496528604,-1.19312375741313,-1.18752804544374,-1.18485054075049,
-1.18272911148411,-1.18007925110546,-1.17462928826426,-1.14659570558973,
-1.11979609484233,-1.10454601711322,-1.09881849975883,-1.09528795179867,
-1.09142627359652,-1.08602448626551,-1.07204197353568,-1.04961711990649,
-1.01439200502626,-1.00946749841059,-1.00688989526563,-1.00478570579984,
-1.00203736967785,-0.996057649487697,-0.987612828446478,-0.961027674378112,
-0.928995314272646,-0.922189678648912,-0.91804561900955,-0.914245962646039,
-0.909233395123018,-0.897854058863521,-0.881449779753469,-0.873478405681935,
-0.839723164020809,-0.832837778243438,-0.830132965077558,-0.827965937935453,
-0.825638057805196,-0.821751750741515,-0.805301727632524,-0.763004484872936,
-0.748692243702467,-0.743093060912541,-0.739584695251194,-0.735701591510242,
-0.730181270271251,-0.715299877918116,-0.690435483761497,-0.659378742363925,
-0.65405622901202,-0.651430864811441,-0.64930889866142,-0.646605118362785,
-0.640868842698541,-0.632886296918339,-0.609050309072773,-0.57590377349962,
-0.568536528569407,-0.563857748232123,-0.560093882171785,-0.555757095735888,
-0.548026454118691,-0.522661168402109,-0.484088335858775,-0.477248979051107,
-0.474551509223608,-0.472386317805916,-0.470055037896324,-0.466153132787228,
-0.449443075236179,-0.408967283228258,-0.393484502618362,-0.387727799103882,
-0.384192099958015,-0.380334802546535,-0.374958047900295,-0.361158432775706,
-0.33920333043169,-0.303099337412899,-0.298273233190325,-0.295716508079725,
-0.293590177778295,-0.290802973593218,-0.285157208614073),.UNSPECIFIED.);
#1170=B_SPLINE_CURVE_WITH_KNOTS('',3,(#8144,#8145,#8146,#8147,#8148,#8149,
#8150,#8151,#8152,#8153,#8154,#8155,#8156,#8157,#8158,#8159,#8160,#8161,
#8162,#8163,#8164,#8165,#8166,#8167,#8168,#8169,#8170,#8171,#8172,#8173,
#8174,#8175,#8176,#8177,#8178,#8179,#8180,#8181,#8182,#8183,#8184,#8185,
#8186,#8187,#8188,#8189,#8190,#8191,#8192,#8193,#8194,#8195,#8196,#8197,
#8198,#8199,#8200,#8201,#8202,#8203,#8204,#8205,#8206,#8207,#8208,#8209,
#8210,#8211,#8212,#8213,#8214,#8215,#8216,#8217,#8218,#8219,#8220,#8221,
#8222,#8223,#8224,#8225,#8226,#8227,#8228,#8229,#8230,#8231,#8232,#8233,
#8234,#8235,#8236,#8237,#8238,#8239,#8240,#8241,#8242,#8243,#8244,#8245,
#8246,#8247,#8248,#8249,#8250,#8251,#8252,#8253,#8254,#8255,#8256,#8257,
#8258,#8259,#8260,#8261,#8262,#8263,#8264,#8265,#8266,#8267,#8268,#8269,
#8270,#8271,#8272,#8273,#8274,#8275,#8276,#8277,#8278,#8279,#8280,#8281,
#8282,#8283,#8284,#8285,#8286,#8287,#8288,#8289,#8290,#8291,#8292,#8293,
#8294,#8295,#8296,#8297,#8298,#8299,#8300,#8301,#8302,#8303,#8304,#8305,
#8306,#8307,#8308,#8309,#8310,#8311,#8312,#8313,#8314,#8315,#8316,#8317,
#8318,#8319,#8320,#8321,#8322,#8323,#8324,#8325,#8326,#8327,#8328,#8329,
#8330,#8331,#8332,#8333,#8334,#8335,#8336,#8337,#8338,#8339,#8340,#8341),
 .UNSPECIFIED.,.F.,.F.,(4,2,2,2,2,2,2,2,2,2,2,2,2,2,2,2,2,2,2,2,2,2,2,2,
2,2,2,2,2,2,2,2,2,2,2,2,2,2,2,2,2,2,2,2,2,2,2,2,2,2,2,2,2,2,2,2,2,2,2,2,
2,2,2,2,2,2,2,2,2,2,2,2,2,2,2,2,2,2,2,2,2,2,2,2,2,2,2,2,2,2,2,2,2,2,2,2,
2,2,4),(-1.95382075976061,-1.93845052981756,-1.93070666029189,-1.9263675316077,
-1.92260441862345,-1.91793019017277,-1.91057744168998,-1.87653626945298,
-1.8533311845946,-1.84546181664684,-1.83978665309728,-1.83709442962286,
-1.83497298814602,-1.83233759939909,-1.82696219477251,-1.7979812412323,
-1.78360878890008,-1.76673997215926,-1.75513850476569,-1.75009033008937,
-1.74628608926052,-1.74215864511806,-1.7354304806649,-1.70570588671948,
-1.68167068743024,-1.664781094057,-1.66086882214523,-1.65853550021191,-1.65637184638938,
-1.65367981029778,-1.64687273748103,-1.60829409006462,-1.58293891903977,
-1.5752100522226,-1.57087391298388,-1.56711038473087,-1.5624317303758,-1.55506400416146,
-1.52187827217161,-1.49804835775141,-1.49006645882824,-1.4843311693325,
-1.48162771641708,-1.47950594603847,-1.47688072266254,-1.47155818798291,
-1.43163605391564,-1.40818843102222,-1.39862940882099,-1.39393482962389,
-1.39017024089405,-1.38584575380967,-1.37837749865787,-1.3361049276215,
-1.3181039628199,-1.30808392023966,-1.30474738504513,-1.30253728859641,
-1.30023722684789,-1.29647817865237,-1.28329662560233,-1.25451791384796,
-1.22774616453828,-1.21982779866319,-1.215452848043,-1.21169235392893,-1.20706448124509,
-1.1998714580494,-1.16155001968581,-1.1412710393405,-1.13050817446906,-1.12708839749912,
-1.12486126850819,-1.12285967406226,-1.11946664468586,-1.10894779060463,
-1.08944157058243,-1.04989373171123,-1.04211574409565,-1.0377242011372,
-1.03396476539228,-1.02935756144726,-1.02026350460516,-0.986049149790715,
-0.956172483798929,-0.950819091201227,-0.948187847482847,-0.946066168697338,
-0.943369124946128,-0.937668613180446,-0.92975293161244,-0.906289133856426,
-0.872640417009587,-0.865281885519018,-0.860605785529775,-0.856842305984083,
-0.85250400955929,-0.844765207762263,-0.834941232871745),.UNSPECIFIED.);
#1171=B_SPLINE_CURVE_WITH_KNOTS('',3,(#8343,#8344,#8345,#8346,#8347,#8348,
#8349,#8350,#8351,#8352,#8353,#8354,#8355,#8356,#8357,#8358,#8359,#8360,
#8361,#8362,#8363,#8364,#8365,#8366,#8367,#8368,#8369,#8370,#8371,#8372,
#8373,#8374,#8375,#8376,#8377,#8378,#8379,#8380,#8381,#8382,#8383,#8384,
#8385,#8386,#8387,#8388,#8389,#8390,#8391,#8392,#8393,#8394,#8395,#8396),
 .UNSPECIFIED.,.F.,.F.,(4,2,2,2,2,2,2,2,2,2,2,2,2,2,2,2,2,2,2,2,2,2,2,2,
2,2,4),(-0.285157208614073,-0.284605315737705,-0.275737691792264,-0.246338366236847,
-0.217633348387182,-0.210948205204423,-0.206829394393677,-0.203021468104304,
-0.197950906522848,-0.186213318125285,-0.169054758634776,-0.157029278777212,
-0.126021054712905,-0.120709481011801,-0.118086144868309,-0.11596398705953,
-0.113257637150128,-0.107508001161571,-0.0995005129755145,-0.0681711636269896,
-0.041713286785829,-0.0341178041145199,-0.0297652273629336,-0.0260024939904901,
-0.0223858321731088,-0.0178186478765722,-0.000525515565460478),
 .UNSPECIFIED.);
#1172=B_SPLINE_CURVE_WITH_KNOTS('',3,(#8397,#8398,#8399,#8400,#8401,#8402,
#8403,#8404,#8405,#8406,#8407,#8408,#8409,#8410,#8411,#8412,#8413,#8414,
#8415,#8416,#8417,#8418,#8419,#8420,#8421,#8422,#8423,#8424,#8425,#8426,
#8427,#8428,#8429,#8430,#8431,#8432,#8433,#8434,#8435,#8436,#8437,#8438,
#8439,#8440,#8441,#8442,#8443,#8444,#8445,#8446,#8447,#8448,#8449,#8450,
#8451,#8452,#8453,#8454,#8455,#8456,#8457,#8458,#8459,#8460,#8461,#8462,
#8463,#8464,#8465,#8466,#8467,#8468,#8469,#8470,#8471,#8472,#8473,#8474,
#8475,#8476,#8477,#8478,#8479,#8480,#8481,#8482,#8483,#8484,#8485,#8486,
#8487,#8488,#8489,#8490,#8491,#8492,#8493,#8494,#8495,#8496,#8497,#8498,
#8499,#8500,#8501,#8502,#8503,#8504,#8505,#8506,#8507,#8508,#8509,#8510,
#8511,#8512,#8513,#8514,#8515,#8516,#8517,#8518,#8519,#8520,#8521,#8522,
#8523,#8524,#8525,#8526,#8527,#8528,#8529,#8530,#8531,#8532,#8533,#8534,
#8535,#8536,#8537,#8538,#8539,#8540,#8541,#8542,#8543,#8544,#8545,#8546,
#8547,#8548),.UNSPECIFIED.,.F.,.F.,(4,2,2,2,2,2,2,2,2,2,2,2,2,2,2,2,2,2,
2,2,2,2,2,2,2,2,2,2,2,2,2,2,2,2,2,2,2,2,2,2,2,2,2,2,2,2,2,2,2,2,2,2,2,2,
2,2,2,2,2,2,2,2,2,2,2,2,2,2,2,2,2,2,2,2,2,4),(-2.23842674530037,-2.20180201490224,
-2.18966994179993,-2.18192756901689,-2.17889073702879,-2.1767349235105,
-2.17432599390694,-2.17006282288876,-2.14365978257604,-2.12285723952658,
-2.10716807487443,-2.09953432254986,-2.09323023706848,-2.09302700584519,
-2.09282456983365,-2.09262050856384,-2.09241219277337,-2.08866215051524,
-2.08482843299966,-2.08022266103576,-2.06905290959127,-2.02984685376578,
-2.00837808613535,-2.00308041128917,-2.00045994455024,-1.99854960340612,
-1.99595162979262,-1.99092979930649,-1.95674749436908,-1.94783644870737,
-1.93052176089478,-1.91871064319739,-1.91362873843839,-1.90981944432645,
-1.90570596167661,-1.89904502981321,-1.87151371487476,-1.84723891346056,
-1.83451667686,-1.82651825573437,-1.8234438934767,-1.82128203565596,-1.81888972428875,
-1.81470447929034,-1.79340993024457,-1.76009267369779,-1.74841109768661,
-1.7395040000213,-1.73493266790465,-1.73154005437192,-1.72725699531547,
-1.71997897385422,-1.67629271449942,-1.65902775150732,-1.64926296056025,
-1.64595642957898,-1.6437522395154,-1.64144330613434,-1.63764372435906,
-1.62428903489381,-1.58405022798349,-1.56522856919212,-1.55927063913065,
-1.55530274281241,-1.55146139176783,-1.54682467369087,-1.53775892958849,
-1.49709094362333,-1.4751436430194,-1.46979416645313,-1.4671636272084,-1.46525279678868,
-1.46266419502246,-1.45768717370014,-1.42300963777067,-1.40408768184211),
 .UNSPECIFIED.);
#1173=B_SPLINE_CURVE_WITH_KNOTS('',3,(#8554,#8555,#8556,#8557,#8558,#8559,
#8560,#8561,#8562,#8563,#8564,#8565,#8566,#8567,#8568,#8569,#8570,#8571,
#8572,#8573,#8574,#8575,#8576,#8577,#8578,#8579,#8580,#8581,#8582,#8583,
#8584,#8585,#8586,#8587,#8588,#8589,#8590,#8591,#8592,#8593,#8594,#8595,
#8596,#8597,#8598,#8599,#8600,#8601,#8602,#8603,#8604,#8605,#8606,#8607,
#8608,#8609,#8610,#8611,#8612,#8613,#8614,#8615,#8616,#8617,#8618,#8619,
#8620,#8621,#8622,#8623,#8624,#8625,#8626,#8627,#8628,#8629,#8630,#8631,
#8632,#8633,#8634,#8635,#8636,#8637,#8638,#8639,#8640,#8641,#8642,#8643,
#8644,#8645,#8646,#8647,#8648,#8649,#8650,#8651,#8652,#8653,#8654,#8655,
#8656,#8657,#8658,#8659,#8660,#8661,#8662,#8663,#8664,#8665,#8666,#8667,
#8668,#8669,#8670,#8671,#8672,#8673,#8674,#8675,#8676,#8677,#8678,#8679,
#8680,#8681,#8682,#8683,#8684,#8685,#8686,#8687,#8688,#8689,#8690,#8691),
 .UNSPECIFIED.,.F.,.F.,(4,2,2,2,2,2,2,2,2,2,2,2,2,2,2,2,2,2,2,2,2,2,2,2,
2,2,2,2,2,2,2,2,2,2,2,2,2,2,2,2,2,2,2,2,2,2,2,2,2,2,2,2,2,2,2,2,2,2,2,2,
2,2,2,2,2,2,2,2,4),(-0.835256000403932,-0.833903157656945,-0.812359280303279,
-0.772906016290568,-0.761742991407092,-0.756819852231102,-0.753020966189164,
-0.748875386505999,-0.742061750144066,-0.733846448660133,-0.716225295331351,
-0.682393038555207,-0.670960543256474,-0.667361518401213,-0.665096077698588,
-0.662858079276838,-0.659386957525091,-0.648136065023465,-0.626234021226254,
-0.590393904725122,-0.583084292388291,-0.578422273186637,-0.57465956001657,
-0.570310446477138,-0.562519521086389,-0.536709477564335,-0.495947463558973,
-0.490778944313391,-0.488183563551013,-0.486272866385113,-0.483649047011384,
-0.478335014037764,-0.45671853228855,-0.417047993935379,-0.406088929278421,
-0.401199285081014,-0.397404873973042,-0.393242635400209,-0.386350500761623,
-0.350929340560522,-0.318142757303684,-0.312975191761013,-0.310379966516739,
-0.308469219822453,-0.30584512450112,-0.300529844484094,-0.278902452756725,
-0.239199500931647,-0.228409066348316,-0.223473713458805,-0.219672820778468,
-0.215532442801598,-0.208744651543829,-0.172782084351853,-0.140380215201286,
-0.135184352332277,-0.132583528116008,-0.130672982466842,-0.128054645602272,
-0.123348883316926,-0.110283297282169,-0.0704009510092085,-0.0529433306947419,
-0.0469698863250932,-0.0433951641945868,-0.0395659255329625,-0.0357922251787191,
-0.030736217758438,-0.000525840699380102),.UNSPECIFIED.);
#1174=B_SPLINE_CURVE_WITH_KNOTS('',3,(#8692,#8693,#8694,#8695,#8696,#8697,
#8698,#8699,#8700,#8701,#8702,#8703,#8704,#8705,#8706,#8707,#8708,#8709,
#8710,#8711,#8712,#8713,#8714,#8715,#8716,#8717,#8718,#8719,#8720,#8721,
#8722,#8723,#8724,#8725,#8726,#8727,#8728,#8729,#8730,#8731,#8732,#8733,
#8734,#8735,#8736,#8737,#8738,#8739,#8740,#8741,#8742,#8743,#8744,#8745,
#8746,#8747,#8748,#8749,#8750,#8751,#8752,#8753,#8754,#8755,#8756,#8757,
#8758,#8759,#8760,#8761,#8762,#8763),.UNSPECIFIED.,.F.,.F.,(4,2,2,2,2,2,
2,2,2,2,2,2,2,2,2,2,2,2,2,2,2,2,2,2,2,2,2,2,2,2,2,2,2,2,2,4),(-2.23817129971403,
-2.20004353776308,-2.19641612000517,-2.19328204071144,-2.19111031208694,
-2.18874301483652,-2.18467310509577,-2.16661948324098,-2.13761835312644,
-2.11379425744401,-2.10749510880762,-2.10730306054185,-2.10710989232745,
-2.10691338764266,-2.10671107509834,-2.10650008085897,-2.1062769239631,
-2.10603721756826,-2.10577521164799,-2.10548305860718,-2.10514957058804,
-2.10489058491089,-2.10424380038591,-2.10048369441894,-2.0958552735416,
-2.08865934590121,-2.04245770713627,-2.02764573932396,-2.02159127472162,
-2.01693354826721,-2.01444164074152,-2.01230682513711,-2.0094754871114,
-2.00310539243814,-1.96391664450224,-1.95382075976061),.UNSPECIFIED.);
#1175=B_SPLINE_CURVE_WITH_KNOTS('',3,(#8764,#8765,#8766,#8767,#8768,#8769,
#8770,#8771,#8772,#8773,#8774,#8775,#8776,#8777,#8778,#8779,#8780,#8781,
#8782,#8783,#8784,#8785,#8786,#8787,#8788,#8789,#8790,#8791,#8792,#8793,
#8794,#8795,#8796,#8797,#8798,#8799,#8800,#8801,#8802,#8803,#8804,#8805,
#8806,#8807,#8808,#8809,#8810,#8811,#8812,#8813,#8814,#8815,#8816,#8817,
#8818,#8819,#8820,#8821,#8822,#8823,#8824,#8825,#8826,#8827,#8828,#8829,
#8830,#8831,#8832,#8833,#8834,#8835,#8836,#8837,#8838,#8839,#8840,#8841,
#8842,#8843,#8844,#8845,#8846,#8847,#8848,#8849,#8850,#8851,#8852,#8853,
#8854,#8855,#8856,#8857,#8858,#8859,#8860,#8861,#8862,#8863,#8864,#8865,
#8866,#8867,#8868,#8869,#8870,#8871,#8872,#8873,#8874,#8875,#8876,#8877,
#8878,#8879,#8880,#8881,#8882,#8883,#8884,#8885,#8886,#8887,#8888,#8889,
#8890,#8891,#8892,#8893,#8894,#8895,#8896,#8897,#8898,#8899,#8900,#8901,
#8902,#8903,#8904,#8905,#8906,#8907,#8908,#8909,#8910,#8911,#8912,#8913,
#8914,#8915,#8916,#8917,#8918,#8919,#8920,#8921,#8922,#8923,#8924,#8925,
#8926,#8927,#8928,#8929,#8930,#8931,#8932,#8933,#8934,#8935,#8936,#8937,
#8938,#8939,#8940,#8941,#8942,#8943,#8944,#8945,#8946,#8947,#8948,#8949,
#8950,#8951),.UNSPECIFIED.,.F.,.F.,(4,2,2,2,2,2,2,2,2,2,2,2,2,2,2,2,2,2,
2,2,2,2,2,2,2,2,2,2,2,2,2,2,2,2,2,2,2,2,2,2,2,2,2,2,2,2,2,2,2,2,2,2,2,2,
2,2,2,2,2,2,2,2,2,2,2,2,2,2,2,2,2,2,2,2,2,2,2,2,2,2,2,2,2,2,2,2,2,2,2,2,
2,2,2,4),(-1.40408768184211,-1.38957977527783,-1.38254760910776,-1.37835622038408,
-1.37456965438362,-1.36973754043997,-1.3591190653567,-1.31906290772079,
-1.29731495573317,-1.29198685823671,-1.2893604235364,-1.28744974902084,
-1.28485721287769,-1.27986161632148,-1.24537782625693,-1.21126940426693,
-1.20450717764904,-1.20037242202396,-1.1965702310934,-1.1916239938707,-1.18031973079987,
-1.14098594949752,-1.11947709763186,-1.11417486586332,-1.11155342246128,
-1.10943131033475,-1.10672313102682,-1.10096316874451,-1.09293611811218,
-1.06884840798944,-1.0360422700045,-1.02867043304112,-1.02399029516852,
-1.0202262993262,-1.01589042278099,-1.00816435230079,-0.982832809034957,
-0.944442070007762,-0.937444759403386,-0.934722432697565,-0.932550910248748,
-0.930230787290733,-0.926380329303665,-0.910504634429364,-0.861634803291888,
-0.851423795062694,-0.846593799721364,-0.842807469332458,-0.838614872327558,
-0.831577128402275,-0.798030270312757,-0.763460252719972,-0.758469500754523,
-0.755877960791643,-0.75396719045863,-0.751339592492114,-0.746005635888466,
-0.724203683294803,-0.683969226260979,-0.67353866940251,-0.6686868917186,
-0.664907439052627,-0.660682198025089,-0.653488882022884,-0.620090225590341,
-0.585684345425944,-0.580678345683627,-0.578083572752282,-0.576172914840194,
-0.573548641816458,-0.568232018779985,-0.546591071032606,-0.506847054563397,
-0.495957227979738,-0.491079219077355,-0.487286486230984,-0.483118639850554,
-0.476199400510116,-0.441314198016256,-0.408004105087279,-0.40286079443622,
-0.400270399084497,-0.398359485125245,-0.395730433497096,-0.390389313661894,
-0.368521952510856,-0.328087975161761,-0.317838832645986,-0.313018842471736,
-0.30924265359313,-0.304998730755654,-0.297716530745075,-0.288760759917401,
-0.284919832709406),.UNSPECIFIED.);
#1176=B_SPLINE_CURVE_WITH_KNOTS('',3,(#8956,#8957,#8958,#8959,#8960,#8961,
#8962,#8963,#8964,#8965,#8966,#8967,#8968,#8969,#8970,#8971,#8972,#8973,
#8974,#8975,#8976,#8977,#8978,#8979,#8980,#8981,#8982,#8983,#8984,#8985,
#8986,#8987,#8988,#8989,#8990,#8991,#8992,#8993,#8994,#8995,#8996,#8997,
#8998,#8999,#9000,#9001,#9002,#9003,#9004,#9005,#9006,#9007,#9008,#9009,
#9010,#9011,#9012,#9013,#9014,#9015,#9016,#9017,#9018,#9019,#9020,#9021,
#9022,#9023,#9024,#9025,#9026,#9027,#9028,#9029,#9030,#9031,#9032,#9033,
#9034,#9035,#9036,#9037,#9038,#9039,#9040,#9041,#9042,#9043,#9044,#9045,
#9046,#9047,#9048,#9049,#9050,#9051,#9052,#9053,#9054,#9055,#9056,#9057,
#9058,#9059,#9060,#9061,#9062,#9063,#9064,#9065,#9066,#9067,#9068,#9069,
#9070,#9071,#9072,#9073,#9074,#9075,#9076,#9077,#9078,#9079,#9080,#9081,
#9082,#9083,#9084,#9085,#9086,#9087,#9088,#9089,#9090,#9091,#9092,#9093,
#9094,#9095,#9096,#9097,#9098,#9099,#9100,#9101,#9102,#9103,#9104,#9105,
#9106,#9107,#9108,#9109,#9110,#9111,#9112,#9113,#9114,#9115,#9116,#9117,
#9118,#9119,#9120,#9121,#9122,#9123,#9124,#9125,#9126,#9127,#9128,#9129,
#9130,#9131,#9132,#9133,#9134,#9135,#9136,#9137,#9138,#9139,#9140,#9141,
#9142,#9143),.UNSPECIFIED.,.F.,.F.,(4,2,2,2,2,2,2,2,2,2,2,2,2,2,2,2,2,2,
2,2,2,2,2,2,2,2,2,2,2,2,2,2,2,2,2,2,2,2,2,2,2,2,2,2,2,2,2,2,2,2,2,2,2,2,
2,2,2,2,2,2,2,2,2,2,2,2,2,2,2,2,2,2,2,2,2,2,2,2,2,2,2,2,2,2,2,2,2,2,2,2,
2,2,2,4),(-1.95425084573748,-1.9488048353452,-1.9265034475259,-1.91880226621803,
-1.91321778982713,-1.91054292250933,-1.90842225940067,-1.90577172519139,
-1.90031504000988,-1.8750307949933,-1.85220842069598,-1.83119200737488,
-1.82504133564151,-1.82103505619071,-1.81722087565314,-1.81186587393905,
-1.80200383315236,-1.75851717974032,-1.73854180639263,-1.73447773956142,
-1.73211188553927,-1.72996434008032,-1.72684631381955,-1.71909579802802,
-1.68610940505473,-1.65630212209218,-1.64864835940714,-1.64432788703489,
-1.640563121571,-1.63586350133981,-1.62627648002117,-1.58509586145795,-1.56103132328574,
-1.55683423800556,-1.55443942553061,-1.55227861322663,-1.54921024303087,
-1.54179666366109,-1.5085179681387,-1.47679903864488,-1.47008918832085,
-1.46596571971358,-1.46216038813747,-1.45719065976957,-1.44620273467432,
-1.40669390553267,-1.38512791039511,-1.3798198289021,-1.37719743252561,
-1.3752871143026,-1.37269126461299,-1.36751898869572,-1.32681405945243,
-1.30100383799497,-1.29321337380989,-1.28886472298043,-1.28510249963056,
-1.2804412072163,-1.27136734789151,-1.22083982450515,-1.20482486924466,
-1.20096545513965,-1.19864348717774,-1.1964732106804,-1.19375553389689,
-1.18678848318401,-1.1396272115232,-1.11983545923122,-1.11378764292675,
-1.10980145032778,-1.1059283898753,-1.1004625781689,-1.08600083173267,-1.06230310826659,
-1.02927012023504,-1.02411505750058,-1.02152245033762,-1.01961178474448,
-1.01698545049361,-1.01165776158438,-0.98991279172966,-0.949850183639881,
-0.939263623961265,-0.934437007517011,-0.930651131653822,-0.926456766650751,
-0.919410460722941,-0.885650264324294,-0.851353532017681,-0.846338411659938,
-0.843741777320511,-0.841831267552231,-0.839209116342534,-0.835256000403932),
 .UNSPECIFIED.);
#1177=B_SPLINE_CURVE_WITH_KNOTS('',3,(#9145,#9146,#9147,#9148,#9149,#9150,
#9151,#9152,#9153,#9154,#9155,#9156,#9157,#9158,#9159,#9160,#9161,#9162,
#9163,#9164,#9165,#9166,#9167,#9168,#9169,#9170,#9171,#9172,#9173,#9174,
#9175,#9176,#9177,#9178,#9179,#9180,#9181,#9182,#9183,#9184,#9185,#9186,
#9187,#9188,#9189,#9190,#9191,#9192,#9193,#9194),.UNSPECIFIED.,.F.,.F.,
(4,2,2,2,2,2,2,2,2,2,2,2,2,2,2,2,2,2,2,2,2,2,2,2,4),(-0.284919832709406,
-0.268478615398321,-0.237573699351308,-0.22723363851388,-0.223759085365556,
-0.221741974625486,-0.219530950620218,-0.216190734162257,-0.206140542589294,
-0.188053575860309,-0.145918927656313,-0.138458189823389,-0.134135025753909,
-0.130369802853748,-0.125672100899879,-0.116422632003618,-0.103919850873366,
-0.0706983448033028,-0.0507324000467649,-0.0465906968120399,-0.0442076003520664,
-0.0420418358083735,-0.0389449114566336,-0.0353734051747675,-0.000526036917278915),
 .UNSPECIFIED.);
#1178=B_SPLINE_CURVE_WITH_KNOTS('',3,(#9195,#9196,#9197,#9198,#9199,#9200,
#9201,#9202,#9203,#9204,#9205,#9206,#9207,#9208,#9209,#9210,#9211,#9212,
#9213,#9214,#9215,#9216,#9217,#9218,#9219,#9220,#9221,#9222,#9223,#9224,
#9225,#9226,#9227,#9228,#9229,#9230,#9231,#9232,#9233,#9234,#9235,#9236,
#9237,#9238,#9239,#9240,#9241,#9242,#9243,#9244,#9245,#9246,#9247,#9248,
#9249,#9250,#9251,#9252,#9253,#9254,#9255,#9256,#9257,#9258,#9259,#9260,
#9261,#9262,#9263,#9264,#9265,#9266,#9267,#9268,#9269,#9270,#9271,#9272,
#9273,#9274,#9275,#9276,#9277,#9278,#9279,#9280,#9281,#9282,#9283,#9284,
#9285,#9286,#9287,#9288,#9289,#9290,#9291,#9292,#9293,#9294,#9295,#9296,
#9297,#9298,#9299,#9300,#9301,#9302,#9303,#9304,#9305,#9306,#9307,#9308,
#9309,#9310,#9311,#9312,#9313,#9314,#9315,#9316,#9317,#9318,#9319,#9320,
#9321,#9322,#9323,#9324,#9325,#9326,#9327,#9328,#9329,#9330,#9331,#9332,
#9333),.UNSPECIFIED.,.F.,.F.,(4,3,3,3,3,3,3,3,3,3,3,3,3,3,3,3,3,3,3,3,3,
3,3,3,3,3,3,3,3,3,3,3,3,3,3,3,3,3,3,3,3,3,3,3,3,3,4),(84.8230016469243,
84.9294800319919,85.035885845196,85.1422596419165,85.2510514517916,85.3575496036659,
85.4674882425415,85.577426881417,85.6854677190469,85.7967369523817,85.9044808232374,
86.0121588393832,86.1198098017914,86.2274724668646,86.3352547121903,86.443109349129,
86.5511458411805,86.5756215857255,86.683662473221,86.7949317003226,86.9026756201591,
87.0103536848308,87.1180046952373,87.2256674077084,87.3334496992533,87.4413043817755,
87.5493409180866,87.573816290034,87.6818572432399,87.7931264621277,87.9008704494791,
88.0085485821443,88.1161996609114,88.2238624419986,88.3316448020907,88.4394995531984,
88.54753615753,88.5720109943425,88.6800561759704,88.787908823887,88.8956535691258,
89.0033293074333,89.1109748434047,89.2186917097602,89.3264442868578,89.4343611966998,
89.5083060834268),.UNSPECIFIED.);
#1179=B_SPLINE_CURVE_WITH_KNOTS('',3,(#9339,#9340,#9341,#9342,#9343,#9344,
#9345,#9346,#9347),.UNSPECIFIED.,.F.,.F.,(4,1,1,1,1,1,4),(91.106186954104,
91.2534425448399,92.2516372491484,93.2498319534569,94.2480266577654,95.2462213620739,
95.7916382276144),.UNSPECIFIED.);
#1180=B_SPLINE_CURVE_WITH_KNOTS('',3,(#9348,#9349,#9350,#9351,#9352,#9353,
#9354,#9355,#9356,#9357,#9358,#9359,#9360,#9361,#9362,#9363,#9364,#9365,
#9366,#9367,#9368,#9369,#9370,#9371,#9372,#9373,#9374,#9375,#9376,#9377,
#9378,#9379,#9380,#9381,#9382,#9383,#9384,#9385,#9386,#9387,#9388,#9389,
#9390,#9391,#9392,#9393),.UNSPECIFIED.,.F.,.F.,(4,2,2,2,2,2,2,2,2,2,2,2,
2,2,2,2,2,2,2,2,2,2,4),(-2.23890486318736,-2.1921187183875,-2.18288919550491,
-2.17825630531376,-2.17449557784802,-2.17012462176104,-2.16244206011508,
-2.11530710916638,-2.10089665912402,-2.0949452096968,-2.09051708649427,
-2.08819902923615,-2.08628795447926,-2.08370254441095,-2.07858266815642,
-2.03764433987988,-2.01197095058656,-2.00419975052637,-1.99985546585281,
-1.99609348737935,-1.99142792657138,-1.98410364382918,-1.95425084573748),
 .UNSPECIFIED.);
#1181=B_SPLINE_CURVE_WITH_KNOTS('',3,(#9395,#9396,#9397,#9398,#9399,#9400,
#9401,#9402,#9403,#9404,#9405,#9406,#9407,#9408,#9409,#9410,#9411,#9412,
#9413,#9414,#9415,#9416,#9417,#9418,#9419,#9420,#9421,#9422,#9423,#9424,
#9425,#9426,#9427,#9428,#9429,#9430,#9431,#9432,#9433,#9434,#9435,#9436,
#9437,#9438,#9439,#9440,#9441,#9442,#9443),.UNSPECIFIED.,.F.,.F.,(4,3,3,
3,3,3,3,3,3,3,3,3,3,3,3,3,4),(89.5083060834268,89.570205698651,89.6782467845126,
89.7895159868185,89.8972601001135,90.0049383559305,90.1125895548881,90.2202524530328,
90.3280349248704,90.4358897847461,90.5439264925945,90.5684004029595,90.6802091645352,
90.7917344437616,90.9030923633481,91.0142725525455,91.106186954104),
 .UNSPECIFIED.);
#1182=B_SPLINE_CURVE_WITH_KNOTS('',3,(#9444,#9445,#9446,#9447,#9448,#9449,
#9450,#9451,#9452),.UNSPECIFIED.,.F.,.F.,(4,1,1,1,1,1,4),(91.106189856623,
91.566595107268,92.5647898115765,93.562984515885,94.5611792201935,95.559373924502,
95.7927227292494),.UNSPECIFIED.);
#1183=B_SPLINE_CURVE_WITH_KNOTS('',3,(#9460,#9461,#9462,#9463,#9464,#9465),
 .UNSPECIFIED.,.F.,.F.,(4,1,1,4),(0.,0.998194704308485,1.99638940861699,
2.31370279205594),.UNSPECIFIED.);
#1184=B_SPLINE_CURVE_WITH_KNOTS('',3,(#9467,#9468,#9469,#9470,#9471,#9472,
#9473,#9474,#9475,#9476,#9477,#9478,#9479,#9480,#9481,#9482,#9483,#9484,
#9485,#9486,#9487,#9488,#9489,#9490,#9491,#9492,#9493,#9494,#9495,#9496,
#9497,#9498,#9499,#9500,#9501,#9502,#9503,#9504,#9505,#9506,#9507,#9508,
#9509,#9510,#9511,#9512,#9513,#9514,#9515,#9516,#9517,#9518,#9519,#9520,
#9521,#9522,#9523,#9524,#9525,#9526,#9527,#9528,#9529,#9530,#9531,#9532,
#9533,#9534,#9535,#9536,#9537,#9538,#9539,#9540,#9541,#9542,#9543,#9544,
#9545,#9546,#9547,#9548,#9549,#9550,#9551,#9552,#9553,#9554,#9555,#9556,
#9557,#9558,#9559,#9560,#9561,#9562,#9563,#9564,#9565,#9566,#9567,#9568,
#9569,#9570,#9571,#9572,#9573,#9574,#9575,#9576,#9577,#9578,#9579,#9580,
#9581,#9582,#9583,#9584,#9585,#9586,#9587,#9588,#9589,#9590,#9591,#9592,
#9593,#9594,#9595,#9596,#9597,#9598,#9599,#9600,#9601,#9602,#9603,#9604,
#9605,#9606,#9607,#9608,#9609,#9610,#9611,#9612,#9613,#9614,#9615,#9616,
#9617,#9618,#9619,#9620,#9621,#9622,#9623,#9624,#9625,#9626,#9627,#9628,
#9629,#9630,#9631,#9632,#9633,#9634,#9635,#9636,#9637,#9638,#9639,#9640,
#9641,#9642,#9643,#9644,#9645,#9646,#9647,#9648,#9649,#9650,#9651,#9652,
#9653,#9654,#9655,#9656),.UNSPECIFIED.,.F.,.F.,(4,3,3,3,3,3,3,3,3,3,3,3,
3,3,3,3,3,3,3,3,3,3,3,3,3,3,3,3,3,3,3,3,3,3,3,3,3,3,3,3,3,3,3,3,3,3,3,3,
3,3,3,3,3,3,3,3,3,3,3,3,3,3,3,4),(2.31370765917172,2.41522060882339,2.51670184339182,
2.61818497064019,2.71977323634762,2.82141660228884,2.92324139570188,2.99458411292549,
3.09711859878378,3.19950611514853,3.30177834504594,3.40398832525274,3.50616880821478,
3.60835250643925,3.71064239648886,3.8129869464208,3.915514075849,3.99277881723399,
4.09503733104183,4.19714389723365,4.29912907287259,4.40104840137011,4.50293505561395,
4.60482216517742,4.70681324268719,4.80885727804268,4.91108450620713,4.99097352154248,
5.093358017046,5.19559212371012,5.29770656547786,5.3997561560771,5.5017738833334,
5.60379269269114,5.70591553066315,5.80809157024813,5.91044970192135,5.98916822585098,
6.09155363136855,6.19378903128511,6.29590533799785,6.39795714348975,6.49997743318058,
6.60199915045676,6.70412541657074,6.80630517836143,6.90866747705169,6.98736293015948,
7.08971603159645,7.19191852085989,7.2940011652135,7.39601886409793,7.49800465172254,
7.59999151984254,7.70208263861518,7.80422703225764,7.90655400033986,7.98555763446798,
8.08909372668814,8.19246919758474,8.29569493507905,8.39883155622788,8.50192254712059,
8.59689296635125),.UNSPECIFIED.);
#1185=B_SPLINE_CURVE_WITH_KNOTS('',3,(#9658,#9659,#9660,#9661,#9662,#9663,
#9664,#9665,#9666,#9667,#9668,#9669,#9670,#9671,#9672,#9673,#9674,#9675,
#9676,#9677,#9678,#9679,#9680,#9681,#9682,#9683,#9684,#9685,#9686,#9687,
#9688,#9689,#9690,#9691,#9692,#9693,#9694,#9695,#9696,#9697,#9698,#9699,
#9700,#9701,#9702,#9703,#9704,#9705,#9706,#9707,#9708,#9709,#9710,#9711,
#9712,#9713,#9714,#9715,#9716,#9717,#9718,#9719,#9720,#9721,#9722,#9723,
#9724,#9725,#9726,#9727,#9728,#9729,#9730,#9731,#9732,#9733,#9734,#9735,
#9736,#9737,#9738,#9739,#9740,#9741,#9742,#9743,#9744,#9745,#9746,#9747,
#9748,#9749,#9750,#9751,#9752,#9753,#9754,#9755,#9756,#9757,#9758,#9759,
#9760,#9761,#9762,#9763,#9764,#9765,#9766,#9767,#9768,#9769,#9770,#9771,
#9772,#9773,#9774,#9775,#9776,#9777,#9778,#9779,#9780,#9781,#9782,#9783,
#9784,#9785,#9786,#9787,#9788,#9789,#9790,#9791,#9792,#9793,#9794,#9795,
#9796,#9797,#9798,#9799,#9800,#9801,#9802,#9803,#9804,#9805,#9806,#9807,
#9808,#9809,#9810,#9811,#9812,#9813,#9814,#9815,#9816,#9817,#9818,#9819,
#9820,#9821,#9822,#9823,#9824,#9825,#9826,#9827,#9828,#9829,#9830,#9831,
#9832,#9833,#9834,#9835,#9836,#9837,#9838,#9839,#9840,#9841,#9842,#9843,
#9844,#9845,#9846,#9847),.UNSPECIFIED.,.F.,.F.,(4,3,3,3,3,3,3,3,3,3,3,3,
3,3,3,3,3,3,3,3,3,3,3,3,3,3,3,3,3,3,3,3,3,3,3,3,3,3,3,3,3,3,3,3,3,3,3,3,
3,3,3,3,3,3,3,3,3,3,3,3,3,3,3,4),(8.59689296679312,8.71065869504464,8.82488625940654,
8.93970254030743,8.98375233877648,9.08612148663761,9.18834028109337,9.2904395402446,
9.39247403555406,9.49447677718119,9.59648073300154,9.69858902871033,9.80075067590721,
9.90309482774171,9.98194704308498,10.0843125227032,10.1865275760404,10.2886230026925,
10.3906536113638,10.4926524177611,10.5946523952558,10.6967566731526,10.7989142742985,
10.9012543794308,10.9801417473935,11.0825095487835,11.1847269570185,11.2868247768608,
11.3888578010099,11.4908590416982,11.5928614688437,11.6949682032125,11.7971282684864,
11.8994708223271,11.978336451702,12.0807039145387,12.1829209845634,12.2850184683913,
12.3870511580443,12.4890520662475,12.5910541634126,12.6931605740422,12.7953203185295,
12.8976625601372,12.9765311560105,13.0788982177589,13.1811148781567,13.2832119415084,
13.3852442042399,13.4872446796843,13.5892463388556,13.691352306376,13.7935116042178,
13.8958533984137,13.974725860319,14.0758680560039,14.1768398940109,14.2777162292637,
14.3785316339025,14.4793205993077,14.5801813237648,14.6810738307868,14.7821341386101,
14.8800782730761),.UNSPECIFIED.);
#1186=B_SPLINE_CURVE_WITH_KNOTS('',3,(#9849,#9850,#9851,#9852,#9853,#9854,
#9855,#9856,#9857,#9858,#9859,#9860,#9861,#9862,#9863,#9864,#9865,#9866,
#9867,#9868,#9869,#9870,#9871,#9872,#9873,#9874,#9875,#9876,#9877,#9878,
#9879,#9880,#9881,#9882,#9883,#9884,#9885,#9886,#9887,#9888,#9889,#9890,
#9891,#9892,#9893,#9894,#9895,#9896,#9897,#9898,#9899,#9900,#9901,#9902,
#9903,#9904,#9905,#9906,#9907,#9908,#9909,#9910,#9911,#9912,#9913,#9914,
#9915,#9916,#9917,#9918,#9919,#9920,#9921,#9922,#9923,#9924,#9925,#9926,
#9927,#9928,#9929,#9930,#9931,#9932,#9933,#9934,#9935,#9936,#9937,#9938,
#9939,#9940,#9941,#9942,#9943,#9944,#9945,#9946,#9947,#9948,#9949,#9950,
#9951,#9952,#9953,#9954,#9955,#9956,#9957,#9958,#9959,#9960,#9961,#9962,
#9963,#9964,#9965,#9966,#9967,#9968,#9969,#9970,#9971,#9972,#9973,#9974,
#9975,#9976,#9977,#9978,#9979,#9980,#9981,#9982,#9983,#9984,#9985,#9986,
#9987,#9988,#9989,#9990,#9991,#9992,#9993,#9994,#9995,#9996,#9997,#9998,
#9999,#10000,#10001,#10002,#10003,#10004,#10005,#10006,#10007,#10008,#10009,
#10010,#10011,#10012,#10013,#10014,#10015,#10016,#10017,#10018,#10019,#10020,
#10021,#10022,#10023,#10024,#10025,#10026,#10027,#10028,#10029,#10030,#10031,
#10032,#10033,#10034,#10035,#10036,#10037,#10038),.UNSPECIFIED.,.F.,.F.,
(4,3,3,3,3,3,3,3,3,3,3,3,3,3,3,3,3,3,3,3,3,3,3,3,3,3,3,3,3,3,3,3,3,3,3,
3,3,3,3,3,3,3,3,3,3,3,3,3,3,3,3,3,3,3,3,3,3,3,3,3,3,3,3,4),(14.8800782735309,
14.9729205646275,15.0752878658831,15.1775047700189,15.2796020822822,15.3816345969743,
15.4836353270675,15.5856372432181,15.6877434695587,15.78990302765,15.8922450814957,
15.971115268936,16.0734825285195,16.1756993900125,16.27779665838,16.3798291284296,
16.4818298131971,16.5838316834012,16.685937863147,16.7880973742104,16.8904393808467,
16.9693099732445,17.0716772716465,17.1738941725689,17.2759914810917,17.3780239917218,
17.4800247174366,17.5820266288971,17.684132850093,17.7862924027791,17.8886344508497,
17.967504677553,18.0698719653397,18.1720888555592,18.2741861533,18.376218653105,
18.4782193679672,18.5802212685635,18.6823274789533,18.7844870208486,18.8868290582766,
18.9656993818615,19.0680666656384,19.1702835517416,19.2723808452264,19.3744133406915,
19.4764140511363,19.5784159472436,19.6805221530641,19.7826816903382,19.8850237231117,
19.96389408617,20.0662613748044,20.1684782658453,20.2705755643636,20.3726080649186,
20.4746087805025,20.5766106817907,20.6787168928212,20.7808764353296,20.8832184733183,
20.9620887904785,21.1082185625857,21.1632635807104),.UNSPECIFIED.);
#1187=B_SPLINE_CURVE_WITH_KNOTS('',3,(#10040,#10041,#10042,#10043,#10044,
#10045,#10046,#10047,#10048,#10049,#10050,#10051,#10052,#10053,#10054,#10055,
#10056,#10057,#10058,#10059,#10060,#10061,#10062,#10063,#10064,#10065,#10066,
#10067,#10068,#10069,#10070,#10071,#10072,#10073,#10074,#10075,#10076,#10077,
#10078,#10079,#10080,#10081,#10082,#10083,#10084,#10085,#10086,#10087,#10088,
#10089,#10090,#10091,#10092,#10093,#10094,#10095,#10096,#10097,#10098,#10099,
#10100,#10101,#10102,#10103,#10104,#10105,#10106,#10107,#10108,#10109,#10110,
#10111,#10112,#10113,#10114,#10115,#10116,#10117,#10118,#10119,#10120,#10121,
#10122,#10123,#10124,#10125,#10126,#10127,#10128,#10129,#10130,#10131,#10132,
#10133,#10134,#10135,#10136,#10137,#10138,#10139,#10140,#10141,#10142,#10143,
#10144,#10145,#10146,#10147,#10148,#10149,#10150,#10151,#10152,#10153,#10154,
#10155,#10156,#10157,#10158,#10159,#10160,#10161,#10162,#10163,#10164,#10165,
#10166,#10167,#10168,#10169,#10170,#10171,#10172,#10173,#10174,#10175,#10176,
#10177,#10178,#10179,#10180,#10181,#10182,#10183,#10184,#10185,#10186,#10187,
#10188,#10189,#10190,#10191,#10192,#10193,#10194,#10195,#10196,#10197,#10198,
#10199,#10200,#10201,#10202,#10203,#10204,#10205,#10206,#10207,#10208,#10209,
#10210,#10211,#10212,#10213,#10214,#10215,#10216,#10217,#10218,#10219,#10220,
#10221,#10222,#10223,#10224,#10225,#10226,#10227,#10228,#10229),
 .UNSPECIFIED.,.F.,.F.,(4,3,3,3,3,3,3,3,3,3,3,3,3,3,3,3,3,3,3,3,3,3,3,3,
3,3,3,3,3,3,3,3,3,3,3,3,3,3,3,3,3,3,3,3,3,3,3,3,3,3,3,3,3,3,3,3,3,3,3,3,
3,3,3,4),(21.1632635810437,21.263959503826,21.3645711896956,21.4651334149979,
21.5656808869542,21.6663176644117,21.7669966867001,21.8678573289293,21.960283494787,
22.0626507814528,22.1648676704972,22.2669649669871,22.3689974654954,22.4709981790168,
22.5730000782296,22.6751062871795,22.7772658276012,22.8796078635165,22.9584781990955,
23.0608454863558,23.1630623760049,23.265159673112,23.3671921722446,23.4691928863969,
23.5711947862462,23.6733009958367,23.7754605369021,23.8778025734595,23.9566729034039,
24.0590401904257,24.1612570798335,24.2633543766963,24.3653868755827,24.4673875894877,
24.5693894890889,24.6714956984312,24.7736552392482,24.8759972755595,24.9548676077125,
25.0572348947143,25.159451784101,25.2615490809412,25.3635815798042,25.4655822936845,
25.5675841932602,25.669690402576,25.7718499433661,25.8741919796494,25.9530623120209,
26.0554295990936,26.1576464885526,26.2597437854665,26.3617762844044,26.4637769983603,
26.5657788980125,26.6678851074053,26.7700446482726,26.8723866846331,26.9512570163294,
27.0590747241359,27.166577316323,27.2738896157367,27.3809590622594,27.4464488875614),
 .UNSPECIFIED.);
#1188=B_SPLINE_CURVE_WITH_KNOTS('',3,(#10231,#10232,#10233,#10234,#10235,
#10236,#10237,#10238,#10239,#10240,#10241,#10242,#10243,#10244,#10245,#10246,
#10247,#10248,#10249,#10250,#10251,#10252,#10253,#10254,#10255,#10256,#10257,
#10258,#10259,#10260,#10261,#10262,#10263,#10264,#10265,#10266,#10267,#10268,
#10269,#10270,#10271,#10272,#10273,#10274,#10275,#10276,#10277,#10278,#10279,
#10280,#10281,#10282,#10283,#10284,#10285,#10286,#10287,#10288,#10289,#10290,
#10291,#10292,#10293,#10294,#10295,#10296,#10297,#10298,#10299,#10300,#10301,
#10302,#10303,#10304,#10305,#10306,#10307,#10308,#10309,#10310,#10311,#10312,
#10313,#10314,#10315,#10316,#10317,#10318,#10319,#10320,#10321,#10322,#10323,
#10324,#10325,#10326,#10327,#10328,#10329,#10330,#10331,#10332,#10333,#10334,
#10335,#10336,#10337,#10338,#10339,#10340,#10341,#10342,#10343,#10344,#10345,
#10346,#10347,#10348,#10349,#10350,#10351,#10352,#10353,#10354,#10355,#10356,
#10357,#10358,#10359,#10360,#10361,#10362,#10363,#10364,#10365,#10366,#10367,
#10368,#10369,#10370,#10371,#10372,#10373,#10374,#10375,#10376,#10377,#10378,
#10379,#10380,#10381,#10382,#10383,#10384,#10385,#10386,#10387,#10388,#10389,
#10390,#10391,#10392,#10393,#10394,#10395,#10396,#10397,#10398,#10399,#10400,
#10401,#10402,#10403,#10404,#10405,#10406,#10407,#10408,#10409,#10410,#10411,
#10412,#10413,#10414,#10415,#10416,#10417,#10418,#10419,#10420),
 .UNSPECIFIED.,.F.,.F.,(4,3,3,3,3,3,3,3,3,3,3,3,3,3,3,3,3,3,3,3,3,3,3,3,
3,3,3,3,3,3,3,3,3,3,3,3,3,3,3,3,3,3,3,3,3,3,3,3,3,3,3,3,3,3,3,3,3,3,3,3,
3,3,3,4),(27.4464488878901,27.5531138465415,27.660065161629,27.7671651353967,
27.8745554203971,27.9494517206379,28.0518190076774,28.1540358971027,28.2561331939824,
28.3581656928855,28.4601664068066,28.5621683064235,28.6642745157809,28.7664340566127,
28.8687760929379,28.9476464249464,29.0500137119942,29.1522306014279,29.2543278983162,
29.3563603972281,29.458361111158,29.5603630107837,29.66246922015,29.7646287609908,
29.866970797325,29.9458411292549,30.0482084162981,30.1504253057272,30.2525226026107,
30.3545551015178,30.4565558154429,30.5585577150636,30.6606639244251,30.7628234652611,
30.8651655015904,30.9440358335634,31.046403120607,31.1486200100365,31.2507173069205,
31.3527498058281,31.4547505197536,31.5567524193752,31.658858628737,31.7610181695735,
31.8633602059032,31.9422305378719,32.0445978249165,32.146814714347,32.2489120112319,
32.3509445101405,32.452945224067,32.5549471236892,32.6570533330521,32.7592128738895,
32.8615549102202,32.9404252421804,33.0413151814097,33.1420721870169,33.2427311845129,
33.3433269635466,33.443934512472,33.5445428291212,33.6452590321507,33.7296341948134),
 .UNSPECIFIED.);
#1189=B_SPLINE_CURVE_WITH_KNOTS('',3,(#10422,#10423,#10424,#10425,#10426,
#10427,#10428,#10429,#10430,#10431,#10432,#10433,#10434,#10435,#10436,#10437,
#10438,#10439,#10440,#10441,#10442,#10443,#10444,#10445,#10446,#10447,#10448,
#10449,#10450,#10451,#10452,#10453,#10454,#10455,#10456,#10457,#10458,#10459,
#10460,#10461,#10462,#10463,#10464,#10465,#10466,#10467,#10468,#10469,#10470,
#10471,#10472,#10473,#10474,#10475,#10476,#10477,#10478,#10479,#10480,#10481,
#10482,#10483,#10484,#10485,#10486,#10487,#10488,#10489,#10490,#10491,#10492,
#10493,#10494,#10495,#10496,#10497,#10498,#10499,#10500,#10501,#10502,#10503,
#10504,#10505,#10506,#10507,#10508,#10509,#10510,#10511,#10512,#10513,#10514,
#10515,#10516,#10517,#10518,#10519,#10520,#10521,#10522,#10523,#10524,#10525,
#10526,#10527,#10528,#10529,#10530,#10531,#10532,#10533,#10534,#10535,#10536,
#10537,#10538,#10539,#10540,#10541,#10542,#10543,#10544,#10545,#10546,#10547,
#10548,#10549,#10550,#10551,#10552,#10553,#10554,#10555,#10556,#10557,#10558,
#10559,#10560,#10561,#10562,#10563,#10564,#10565,#10566,#10567,#10568,#10569,
#10570,#10571,#10572,#10573,#10574,#10575,#10576,#10577,#10578,#10579,#10580,
#10581,#10582,#10583,#10584,#10585,#10586,#10587,#10588,#10589,#10590,#10591,
#10592,#10593,#10594,#10595,#10596,#10597,#10598,#10599,#10600,#10601,#10602,
#10603,#10604,#10605,#10606,#10607,#10608,#10609,#10610,#10611),
 .UNSPECIFIED.,.F.,.F.,(4,3,3,3,3,3,3,3,3,3,3,3,3,3,3,3,3,3,3,3,3,3,3,3,
3,3,3,3,3,3,3,3,3,3,3,3,3,3,3,3,3,3,3,3,3,3,3,3,3,3,3,3,3,3,3,3,3,3,3,3,
3,3,3,4),(33.7296341950697,33.8730565221767,33.9386199464889,34.040987233533,
34.1432041229628,34.2453014198472,34.3473339187553,34.4493346326813,34.5513365323031,
34.6534427416655,34.7556022825025,34.8579443188328,34.9368146507974,35.0391819378415,
35.1413988272715,35.243496124156,35.345528623064,35.44752933699,35.5495312366119,
35.6516374459743,35.7537969868112,35.8561390231415,35.9350093551059,36.0373766421499,
36.1395935315798,36.2416908284642,36.3437233273722,36.4457240412981,36.5477259409199,
36.6498321502822,36.751991691119,36.8543337274492,36.9332040594144,37.0355713464585,
37.1377882358883,37.2398855327728,37.3419180316808,37.4439187456068,37.5459206452285,
37.6480268545909,37.7501863954277,37.852528431758,37.9313987637229,38.0337660507669,
38.1359829401969,38.2380802370813,38.3401127359893,38.4421134499153,38.5441153495371,
38.6462215588994,38.7483810997363,38.8507231360665,38.9295934680314,39.0319607550755,
39.1341776445054,39.2362749413898,39.3383074402978,39.4403081542238,39.5423100538456,
39.644416263208,39.7465758040449,39.8489178403751,39.9277881723399,40.0128195022493),
 .UNSPECIFIED.);
#1190=B_SPLINE_CURVE_WITH_KNOTS('',3,(#10613,#10614,#10615,#10616,#10617,
#10618,#10619,#10620,#10621,#10622,#10623,#10624,#10625,#10626,#10627,#10628,
#10629,#10630,#10631,#10632,#10633,#10634,#10635,#10636,#10637,#10638,#10639,
#10640,#10641,#10642,#10643,#10644,#10645,#10646,#10647,#10648,#10649,#10650,
#10651,#10652,#10653,#10654,#10655,#10656,#10657,#10658,#10659,#10660,#10661,
#10662,#10663,#10664,#10665,#10666,#10667,#10668,#10669,#10670,#10671,#10672,
#10673,#10674,#10675,#10676,#10677,#10678,#10679,#10680,#10681,#10682,#10683,
#10684,#10685,#10686,#10687,#10688,#10689,#10690,#10691,#10692,#10693,#10694,
#10695,#10696,#10697,#10698,#10699,#10700,#10701,#10702,#10703,#10704,#10705,
#10706,#10707,#10708,#10709,#10710,#10711,#10712,#10713,#10714,#10715,#10716,
#10717,#10718,#10719,#10720,#10721,#10722,#10723,#10724,#10725,#10726,#10727,
#10728,#10729,#10730,#10731,#10732,#10733,#10734,#10735,#10736,#10737,#10738,
#10739,#10740,#10741,#10742,#10743,#10744,#10745,#10746,#10747,#10748,#10749,
#10750,#10751,#10752,#10753,#10754,#10755,#10756,#10757,#10758,#10759,#10760,
#10761,#10762,#10763,#10764,#10765,#10766,#10767,#10768,#10769,#10770,#10771,
#10772,#10773,#10774,#10775,#10776,#10777,#10778,#10779,#10780,#10781,#10782,
#10783,#10784,#10785,#10786,#10787,#10788,#10789,#10790,#10791,#10792,#10793,
#10794,#10795,#10796,#10797,#10798,#10799,#10800,#10801,#10802),
 .UNSPECIFIED.,.F.,.F.,(4,3,3,3,3,3,3,3,3,3,3,3,3,3,3,3,3,3,3,3,3,3,3,3,
3,3,3,3,3,3,3,3,3,3,3,3,3,3,3,3,3,3,3,3,3,3,3,3,3,3,3,3,3,3,3,3,3,3,3,3,
3,3,3,4),(40.0128195026877,40.1139820971137,40.2154821945556,40.3164051406739,
40.4172771797015,40.518132722457,40.6200952610048,40.7210806437024,40.8235317601754,
40.9259828766484,41.0283501636925,41.1305670531224,41.2326643500069,41.334696848915,
41.436697562841,41.5386994624629,41.6408056718253,41.7429652126622,41.8453072489925,
41.9241775809569,42.026544868001,42.1287617574309,42.2308590543154,42.3328915532235,
42.4348922671494,42.5368941667711,42.6390003761335,42.7411599169704,42.8435019533007,
42.9223722852654,43.0247395723094,43.1269564617393,43.2290537586237,43.3310862575318,
43.4330869714578,43.5350888710796,43.6371950804419,43.7393546212787,43.841696657609,
43.9205669895739,44.0229342766178,44.1251511660479,44.2272484629323,44.3292809618403,
44.4312816757661,44.5332835753881,44.6353897847504,44.7375493255873,44.8398913619175,
44.9187616938824,45.0211289809264,45.1233458703563,45.2254431672408,45.3274756661487,
45.4294763800745,45.5314782796963,45.6335844890586,45.7357440298954,45.8380860662257,
45.9169563981909,46.0323952952073,46.1474006819053,46.2616798898559,46.2960048092023),
 .UNSPECIFIED.);
#1191=B_SPLINE_CURVE_WITH_KNOTS('',3,(#10804,#10805,#10806,#10807,#10808,
#10809,#10810,#10811,#10812,#10813,#10814,#10815,#10816,#10817,#10818,#10819,
#10820,#10821,#10822,#10823,#10824,#10825,#10826,#10827,#10828,#10829,#10830,
#10831,#10832,#10833,#10834,#10835,#10836,#10837,#10838,#10839,#10840,#10841,
#10842,#10843,#10844,#10845,#10846,#10847,#10848,#10849,#10850,#10851,#10852,
#10853,#10854,#10855,#10856,#10857,#10858,#10859,#10860,#10861,#10862,#10863,
#10864,#10865,#10866,#10867,#10868,#10869,#10870,#10871,#10872,#10873,#10874,
#10875,#10876,#10877,#10878,#10879,#10880,#10881,#10882,#10883,#10884,#10885,
#10886,#10887,#10888,#10889,#10890,#10891,#10892,#10893,#10894,#10895,#10896,
#10897,#10898,#10899,#10900,#10901,#10902,#10903,#10904,#10905,#10906,#10907,
#10908,#10909,#10910,#10911,#10912,#10913,#10914,#10915,#10916,#10917,#10918,
#10919,#10920,#10921,#10922,#10923,#10924,#10925,#10926,#10927,#10928,#10929,
#10930,#10931,#10932,#10933,#10934,#10935,#10936,#10937,#10938,#10939,#10940,
#10941,#10942,#10943,#10944,#10945,#10946,#10947,#10948,#10949,#10950,#10951,
#10952,#10953,#10954,#10955,#10956,#10957,#10958,#10959,#10960,#10961,#10962,
#10963,#10964,#10965,#10966,#10967,#10968,#10969,#10970,#10971,#10972,#10973,
#10974,#10975,#10976,#10977,#10978,#10979,#10980,#10981,#10982,#10983,#10984,
#10985,#10986,#10987,#10988,#10989,#10990,#10991,#10992,#10993),
 .UNSPECIFIED.,.F.,.F.,(4,3,3,3,3,3,3,3,3,3,3,3,3,3,3,3,3,3,3,3,3,3,3,3,
3,3,3,3,3,3,3,3,3,3,3,3,3,3,3,3,3,3,3,3,3,3,3,3,3,3,3,3,3,3,3,3,3,3,3,3,
3,3,3,4),(46.2960048094288,46.3988769004328,46.5017666821123,46.6051127872091,
46.7081987950647,46.8116749487821,46.9151511024994,47.0175183895434,47.1197352789733,
47.2218325758577,47.3238650747657,47.4258657886916,47.5278676883137,47.629973897676,
47.7321334385129,47.8344754748431,47.9133458068079,48.015713093852,48.1179299832817,
48.2200272801661,48.3220597790741,48.424060493,48.5260623926216,48.628168601984,
48.7303281428208,48.832670179151,48.9115405111164,49.0139077981605,49.1161246875906,
49.218221984475,49.3202544833829,49.4222551973089,49.5242570969307,49.626363306293,
49.7285228471298,49.83086488346,49.9097352154249,50.012102502469,50.1143193918989,
50.2164166887834,50.3184491876915,50.4204499016175,50.5224518012394,50.6245580106018,
50.7267175514387,50.829059587769,50.9079299197334,51.0102972067774,51.1125140962073,
51.2146113930918,51.3166438919998,51.4186446059257,51.5206465055475,51.6227527149098,
51.7249122557464,51.8272542920766,51.9061246240419,52.0082851131966,52.1103000971643,
52.2122030290474,52.3140344574652,52.415822866432,52.5176331112404,52.5791901166084),
 .UNSPECIFIED.);
#1192=B_SPLINE_CURVE_WITH_KNOTS('',3,(#10995,#10996,#10997,#10998,#10999,
#11000,#11001,#11002,#11003,#11004,#11005,#11006,#11007,#11008,#11009,#11010,
#11011,#11012,#11013,#11014,#11015,#11016,#11017,#11018,#11019,#11020,#11021,
#11022,#11023,#11024,#11025,#11026,#11027,#11028,#11029,#11030,#11031,#11032,
#11033,#11034,#11035,#11036,#11037,#11038,#11039,#11040,#11041,#11042,#11043,
#11044,#11045,#11046,#11047,#11048,#11049,#11050,#11051,#11052,#11053,#11054,
#11055,#11056,#11057,#11058,#11059,#11060,#11061,#11062,#11063,#11064,#11065,
#11066,#11067,#11068,#11069,#11070,#11071,#11072,#11073,#11074,#11075,#11076,
#11077,#11078,#11079,#11080,#11081,#11082,#11083,#11084,#11085,#11086,#11087,
#11088,#11089,#11090,#11091,#11092,#11093,#11094,#11095,#11096,#11097,#11098,
#11099,#11100,#11101,#11102,#11103,#11104,#11105,#11106,#11107,#11108,#11109,
#11110,#11111,#11112,#11113,#11114,#11115,#11116,#11117,#11118,#11119,#11120,
#11121,#11122,#11123,#11124,#11125,#11126,#11127,#11128,#11129,#11130,#11131,
#11132,#11133,#11134,#11135,#11136,#11137,#11138,#11139,#11140,#11141,#11142,
#11143,#11144,#11145,#11146,#11147,#11148,#11149,#11150,#11151,#11152,#11153,
#11154,#11155,#11156,#11157,#11158,#11159,#11160,#11161,#11162,#11163,#11164,
#11165,#11166,#11167,#11168,#11169,#11170,#11171,#11172,#11173,#11174,#11175,
#11176,#11177,#11178,#11179,#11180,#11181,#11182,#11183,#11184),
 .UNSPECIFIED.,.F.,.F.,(4,3,3,3,3,3,3,3,3,3,3,3,3,3,3,3,3,3,3,3,3,3,3,3,
3,3,3,3,3,3,3,3,3,3,3,3,3,3,3,3,3,3,3,3,3,3,3,3,3,3,3,3,3,3,3,3,3,3,3,3,
3,3,3,4),(52.5791901170213,52.6988577669334,52.8198639579863,52.9043193283504,
53.006686615395,53.1089035048254,53.2110008017104,53.3130333006189,53.4150340145453,
53.5170359141676,53.6191421235305,53.7213016643679,53.8236437006986,53.9025140326589,
54.0048813197024,54.1070982091317,54.2091955060156,54.3112280049231,54.4132287188485,
54.5152306184698,54.6173368278317,54.719496368668,54.8218384049978,54.9007087369673,
55.0030760240105,55.1052929134395,55.2073902103231,55.3094227092302,55.4114234231553,
55.5134253227762,55.6155315321377,55.7176910729737,55.8200331093031,55.8989034412759,
56.0012707283239,56.1034876177578,56.2055849146462,56.3076174135581,56.409618127488,
56.5116200271138,56.61372623648,56.7158857773207,56.8182278136547,56.8970981455844,
56.9994654326234,57.1016823220481,57.2037796189276,57.3058121178305,57.4078128317515,
57.5098147313683,57.6119209407259,57.714080481558,57.8164225178837,57.8952928498929,
57.9971392720394,58.0988357757483,58.200414347064,58.3019299646778,58.4034163422306,
58.5049071526749,58.6065015936108,58.7081536700367,58.8099768212806,58.8623754235586),
 .UNSPECIFIED.);
#1193=B_SPLINE_CURVE_WITH_KNOTS('',3,(#11186,#11187,#11188,#11189,#11190,
#11191,#11192,#11193,#11194,#11195,#11196,#11197,#11198,#11199,#11200,#11201,
#11202,#11203,#11204,#11205,#11206,#11207,#11208,#11209,#11210,#11211,#11212,
#11213,#11214,#11215,#11216,#11217,#11218,#11219,#11220,#11221,#11222,#11223,
#11224,#11225,#11226,#11227,#11228,#11229,#11230,#11231,#11232,#11233,#11234,
#11235,#11236,#11237,#11238,#11239,#11240,#11241,#11242,#11243,#11244,#11245,
#11246,#11247,#11248,#11249,#11250,#11251,#11252,#11253,#11254,#11255,#11256,
#11257,#11258,#11259,#11260,#11261,#11262,#11263,#11264,#11265,#11266,#11267,
#11268,#11269,#11270,#11271,#11272,#11273,#11274,#11275,#11276,#11277,#11278,
#11279,#11280,#11281,#11282,#11283,#11284,#11285,#11286,#11287,#11288,#11289,
#11290,#11291,#11292,#11293,#11294,#11295,#11296,#11297,#11298,#11299,#11300,
#11301,#11302,#11303,#11304,#11305,#11306,#11307,#11308,#11309,#11310,#11311,
#11312,#11313,#11314,#11315,#11316,#11317,#11318,#11319,#11320,#11321,#11322,
#11323,#11324,#11325,#11326,#11327,#11328,#11329,#11330,#11331,#11332,#11333,
#11334,#11335,#11336,#11337,#11338,#11339,#11340,#11341,#11342,#11343,#11344,
#11345,#11346,#11347,#11348,#11349,#11350,#11351,#11352,#11353,#11354,#11355,
#11356,#11357,#11358,#11359,#11360,#11361,#11362,#11363,#11364,#11365,#11366,
#11367,#11368,#11369,#11370,#11371,#11372,#11373,#11374,#11375),
 .UNSPECIFIED.,.F.,.F.,(4,3,3,3,3,3,3,3,3,3,3,3,3,3,3,3,3,3,3,3,3,3,3,3,
3,3,3,3,3,3,3,3,3,3,3,3,3,3,3,3,3,3,3,3,3,3,3,3,3,3,3,3,3,3,3,3,3,3,3,3,
3,3,3,4),(58.862375423788,58.8934875542014,58.9958548412757,59.0980717307357,
59.2001690276505,59.3022015265887,59.4042022405448,59.5062041401967,59.6083103495887,
59.710469890455,59.8128119268141,59.8916822585099,59.994049545507,60.0962664348901,
60.1983637317282,60.3003962305901,60.4023969444703,60.5043988440467,60.6065050533647,
60.7086645941575,60.811006630445,60.8898769628183,60.9922442498436,61.0944611392541,
61.1965584361184,61.2985909350059,61.4005916489109,61.5025935485113,61.6046997578518,
61.7068592986666,61.8092013349746,61.8880716671269,61.9904389543974,62.0926558440545,
62.1947531411662,62.2967856403013,62.398786354454,62.5007882543017,62.6028944638873,
62.7050540049462,62.8073960414941,62.8862663714353,62.9886336580651,63.0908505470813,
63.1929478435552,63.2949803420546,63.3969810555746,63.4989829547935,63.6010891637607,
63.703248704206,63.805590740155,63.8844610757438,63.9868283627835,64.0890452522045,
64.1911425490737,64.2931750479625,64.3951757618653,64.4971776614602,64.5992838707899,
64.7014434115909,64.8037854478806,64.8826557800523,65.0141082553449,65.1455607306376),
 .UNSPECIFIED.);
#1194=B_SPLINE_CURVE_WITH_KNOTS('',3,(#11377,#11378,#11379,#11380,#11381,
#11382,#11383,#11384,#11385,#11386,#11387,#11388,#11389,#11390,#11391,#11392,
#11393,#11394,#11395,#11396,#11397,#11398,#11399,#11400,#11401,#11402,#11403,
#11404,#11405,#11406,#11407,#11408,#11409,#11410,#11411,#11412,#11413,#11414,
#11415,#11416,#11417,#11418,#11419,#11420,#11421,#11422,#11423,#11424,#11425,
#11426,#11427,#11428,#11429,#11430,#11431,#11432,#11433,#11434,#11435,#11436,
#11437,#11438,#11439,#11440,#11441,#11442,#11443,#11444,#11445,#11446,#11447,
#11448,#11449,#11450,#11451,#11452,#11453,#11454,#11455,#11456,#11457,#11458,
#11459,#11460,#11461,#11462,#11463,#11464,#11465,#11466,#11467,#11468,#11469,
#11470,#11471,#11472,#11473,#11474,#11475,#11476,#11477,#11478,#11479,#11480,
#11481,#11482,#11483,#11484,#11485,#11486,#11487,#11488,#11489,#11490,#11491,
#11492,#11493,#11494,#11495,#11496,#11497,#11498,#11499,#11500,#11501,#11502,
#11503,#11504,#11505,#11506,#11507,#11508,#11509,#11510,#11511,#11512,#11513,
#11514,#11515,#11516,#11517,#11518,#11519,#11520,#11521,#11522,#11523,#11524,
#11525,#11526,#11527,#11528,#11529,#11530,#11531,#11532,#11533,#11534,#11535,
#11536,#11537,#11538,#11539,#11540,#11541,#11542,#11543,#11544,#11545,#11546,
#11547,#11548,#11549,#11550,#11551,#11552,#11553,#11554,#11555,#11556,#11557,
#11558,#11559,#11560,#11561,#11562,#11563,#11564,#11565,#11566,#11567,#11568,
#11569),.UNSPECIFIED.,.F.,.F.,(4,3,3,3,3,3,3,3,3,3,3,3,3,3,3,3,3,3,3,3,
3,3,3,3,3,3,3,3,3,3,3,3,3,3,3,3,3,3,3,3,3,3,3,3,3,3,3,3,3,3,3,3,3,3,3,3,
3,3,3,3,3,3,3,3,4),(65.1455607309676,65.2465970860342,65.3475764640722,
65.4485331628698,65.5495014454226,65.6505785552467,65.7517207397834,65.8530285697123,
65.8808504843608,65.9832177678549,66.0854346537376,66.1875319470962,66.2895644424929,
66.391565152927,66.4935670490809,66.5956732550371,66.6978327924965,66.8001748255344,
66.8790451886693,66.9814124768186,67.0836293673207,67.1857266652233,67.2877591651159,
67.3897598799921,67.4917617805283,67.593867990744,67.6960275324017,67.7983695694907,
67.8772398929778,67.9796071917191,68.0818240929058,68.1839214015799,68.2859539122919,
68.3879546380194,68.4899565494237,68.5920627704566,68.6942223229205,68.7965643706738,
68.8754345972863,68.9778018546988,69.0800187145001,69.1821159818993,69.284148451424,
69.3861491361093,69.4881510066736,69.5902571874619,69.6924166999477,69.7947587086134,
69.8736293015948,69.9759966061904,70.0782135129289,70.1803108266821,70.2823433421819,
70.384344072402,70.4863459879989,70.5884522127361,70.6906117686395,70.7929538193632,
70.8718240059033,70.9770412680876,71.0820752466858,71.1869128579018,71.2916343404495,
71.3962479390824,71.4287460381472),.UNSPECIFIED.);
#1195=B_SPLINE_CURVE_WITH_KNOTS('',3,(#11571,#11572,#11573,#11574,#11575,
#11576,#11577,#11578,#11579,#11580,#11581,#11582,#11583,#11584,#11585,#11586,
#11587,#11588,#11589,#11590,#11591,#11592,#11593,#11594,#11595,#11596,#11597,
#11598,#11599,#11600,#11601,#11602,#11603,#11604,#11605,#11606,#11607,#11608,
#11609,#11610,#11611,#11612,#11613,#11614,#11615,#11616,#11617,#11618,#11619,
#11620,#11621,#11622,#11623,#11624,#11625,#11626,#11627,#11628,#11629,#11630,
#11631,#11632,#11633,#11634,#11635,#11636,#11637,#11638,#11639,#11640,#11641,
#11642,#11643,#11644,#11645,#11646,#11647,#11648,#11649,#11650,#11651,#11652,
#11653,#11654,#11655,#11656,#11657,#11658,#11659,#11660,#11661,#11662,#11663,
#11664,#11665,#11666,#11667,#11668,#11669,#11670,#11671,#11672,#11673,#11674,
#11675,#11676,#11677,#11678,#11679,#11680,#11681,#11682,#11683,#11684,#11685,
#11686,#11687,#11688,#11689,#11690,#11691,#11692,#11693,#11694,#11695,#11696,
#11697,#11698,#11699,#11700,#11701,#11702,#11703,#11704,#11705,#11706,#11707,
#11708,#11709,#11710,#11711,#11712,#11713,#11714,#11715,#11716,#11717,#11718,
#11719,#11720,#11721,#11722,#11723,#11724,#11725,#11726,#11727,#11728,#11729,
#11730,#11731,#11732,#11733,#11734,#11735,#11736,#11737,#11738,#11739,#11740,
#11741,#11742,#11743,#11744,#11745,#11746,#11747,#11748,#11749,#11750,#11751,
#11752,#11753,#11754,#11755,#11756,#11757,#11758,#11759,#11760),
 .UNSPECIFIED.,.F.,.F.,(4,3,3,3,3,3,3,3,3,3,3,3,3,3,3,3,3,3,3,3,3,3,3,3,
3,3,3,3,3,3,3,3,3,3,3,3,3,3,3,3,3,3,3,3,3,3,3,3,3,3,3,3,3,3,3,3,3,3,3,3,
3,3,3,4),(71.4287460384322,71.5390642063771,71.6493304527982,71.7600455583879,
71.8700187102118,71.9723857556817,72.0746024033946,72.1766994594859,72.2787317182815,
72.3807321931089,72.4827338549799,72.5848398303166,72.6869991388247,72.7893409482387,
72.8682134145203,72.9705809069235,73.0727979999874,73.1748954970022,73.2769281938039,
73.3789291031275,73.4809311953892,73.583037591822,73.6851973169359,73.7875395309029,
73.8664081188288,73.9687759209844,74.070993329816,74.1730911499998,74.275124174334,
74.3771254150513,74.4791278420698,74.581234576071,74.6833946408433,74.7857371939683,
74.8646028231373,74.9669681838356,75.0691831445056,75.1712785181177,75.273309098035,
75.3753078999236,75.4773078971386,75.5794122321338,75.6815699111982,75.7839101275024,
75.8627975274458,75.9651669290334,76.0673859212011,76.1694852935143,76.2715198501672,
76.373522601406,76.4755265151415,76.5776346890152,76.6797961699537,76.7821400845837,
76.8609922317543,76.9618586074584,77.0625535278487,77.163152743669,77.2636910931968,
77.3642033289405,77.464774699641,77.5653792250282,77.6661163902905,77.7119313453268),
 .UNSPECIFIED.);
#1196=B_SPLINE_CURVE_WITH_KNOTS('',3,(#11762,#11763,#11764,#11765,#11766,
#11767,#11768,#11769,#11770,#11771),.UNSPECIFIED.,.F.,.F.,(4,1,1,1,1,1,
1,4),(77.7119313453268,77.8591869360628,78.8573816403713,79.8555763446798,
80.8537710489883,81.8519657532968,82.8501604576053,83.7753903812219),
 .UNSPECIFIED.);
#1197=B_SPLINE_CURVE_WITH_KNOTS('',3,(#11775,#11776,#11777,#11778,#11779,
#11780,#11781,#11782,#11783),.UNSPECIFIED.,.F.,.F.,(4,1,1,1,1,1,4),(-85.8447445705308,
-84.8465498662224,-83.8483551619139,-82.8501604576054,-81.8519657532969,
-80.8537710489884,-80.6873799771529),.UNSPECIFIED.);
#1198=B_SPLINE_CURVE_WITH_KNOTS('',3,(#11785,#11786,#11787,#11788,#11789,
#11790,#11791,#11792,#11793,#11794,#11795,#11796,#11797,#11798,#11799,#11800,
#11801,#11802,#11803,#11804,#11805,#11806,#11807,#11808,#11809,#11810,#11811,
#11812,#11813,#11814,#11815,#11816,#11817,#11818,#11819,#11820,#11821,#11822,
#11823,#11824,#11825,#11826,#11827,#11828,#11829,#11830,#11831,#11832,#11833,
#11834,#11835,#11836,#11837,#11838,#11839,#11840,#11841,#11842,#11843,#11844,
#11845,#11846,#11847,#11848,#11849,#11850,#11851,#11852,#11853,#11854,#11855,
#11856,#11857,#11858,#11859,#11860,#11861,#11862,#11863,#11864,#11865,#11866,
#11867,#11868,#11869,#11870,#11871,#11872,#11873,#11874,#11875,#11876,#11877,
#11878,#11879,#11880,#11881,#11882,#11883,#11884,#11885,#11886,#11887,#11888,
#11889,#11890,#11891,#11892,#11893,#11894,#11895,#11896,#11897,#11898,#11899,
#11900,#11901,#11902,#11903,#11904,#11905,#11906,#11907,#11908,#11909,#11910,
#11911,#11912,#11913,#11914,#11915,#11916,#11917,#11918,#11919,#11920,#11921,
#11922,#11923,#11924,#11925,#11926,#11927,#11928,#11929,#11930,#11931,#11932,
#11933,#11934,#11935,#11936,#11937,#11938,#11939,#11940,#11941,#11942,#11943,
#11944,#11945,#11946,#11947,#11948,#11949,#11950,#11951,#11952,#11953,#11954,
#11955,#11956,#11957,#11958,#11959,#11960,#11961,#11962,#11963,#11964,#11965,
#11966,#11967,#11968,#11969,#11970,#11971,#11972,#11973,#11974,#11975,#11976,
#11977),.UNSPECIFIED.,.F.,.F.,(4,3,3,3,3,3,3,3,3,3,3,3,3,3,3,3,3,3,3,3,
3,3,3,3,3,3,3,3,3,3,3,3,3,3,3,3,3,3,3,3,3,3,3,3,3,3,3,3,3,3,3,3,3,3,3,3,
3,3,3,3,3,3,3,3,4),(-80.6873799771529,-80.5834045230938,-80.4828226165599,
-80.3823020159699,-80.2818079446396,-80.1813056668607,-80.0806994109687,
-79.980030174353,-79.8792001208896,-79.8555763446799,-79.7531909320388,
-79.6509555248073,-79.5488392105263,-79.4467873973145,-79.3447670997625,
-79.2427453744942,-79.1406191002387,-79.0384393302107,-78.9360770232174,
-78.8573816403714,-78.7550285516865,-78.6528260753717,-78.5507434441998,
-78.4487257586336,-78.3467399844452,-78.2447531298611,-78.1426620246853,
-78.0405176446954,-77.9381906902025,-77.8591869360629,-77.7568164895759,
-77.65459642229,-77.5524959355451,-77.4504602410313,-77.348456330411,-77.2464512376597,
-77.1443418632008,-77.0421791678361,-76.9398340304818,-76.8609922317544,
-76.7586230828059,-76.6564042872302,-76.5543050269147,-76.4522705304144,
-76.3502677875718,-76.2482638305126,-76.146155533537,-76.0439938850559,
-75.9416497319229,-75.8627975274459,-75.7604320499599,-75.658216998789,
-75.5561215743442,-75.4540909679041,-75.352092163759,-75.2500921885347,
-75.1479879129198,-75.045830314066,-74.9434902112166,-74.8646028231374,
-74.7495007849462,-74.6402031683395,-74.5311448668227,-74.422403289531,
-74.4041946703725),.UNSPECIFIED.);
#1199=B_SPLINE_CURVE_WITH_KNOTS('',3,(#11979,#11980,#11981,#11982,#11983,
#11984,#11985,#11986,#11987,#11988,#11989,#11990,#11991,#11992,#11993,#11994,
#11995,#11996,#11997,#11998,#11999,#12000,#12001,#12002,#12003,#12004,#12005,
#12006,#12007,#12008,#12009,#12010,#12011,#12012,#12013,#12014,#12015,#12016,
#12017,#12018,#12019,#12020,#12021,#12022,#12023,#12024,#12025,#12026,#12027,
#12028,#12029,#12030,#12031,#12032,#12033,#12034,#12035,#12036,#12037,#12038,
#12039,#12040,#12041,#12042,#12043,#12044,#12045,#12046,#12047,#12048,#12049,
#12050,#12051,#12052,#12053,#12054,#12055,#12056,#12057,#12058,#12059,#12060,
#12061,#12062,#12063,#12064,#12065,#12066,#12067,#12068,#12069,#12070,#12071,
#12072,#12073,#12074,#12075,#12076,#12077,#12078,#12079,#12080,#12081,#12082,
#12083,#12084,#12085,#12086,#12087,#12088,#12089,#12090,#12091,#12092,#12093,
#12094,#12095,#12096,#12097,#12098,#12099,#12100,#12101,#12102,#12103,#12104,
#12105,#12106,#12107,#12108,#12109,#12110,#12111,#12112,#12113,#12114,#12115,
#12116,#12117,#12118,#12119,#12120,#12121,#12122,#12123,#12124,#12125,#12126,
#12127,#12128,#12129,#12130,#12131,#12132,#12133,#12134,#12135,#12136,#12137,
#12138,#12139,#12140,#12141,#12142,#12143,#12144,#12145,#12146,#12147,#12148,
#12149,#12150,#12151,#12152,#12153,#12154,#12155,#12156,#12157,#12158,#12159,
#12160,#12161,#12162,#12163,#12164,#12165,#12166,#12167,#12168),
 .UNSPECIFIED.,.F.,.F.,(4,3,3,3,3,3,3,3,3,3,3,3,3,3,3,3,3,3,3,3,3,3,3,3,
3,3,3,3,3,3,3,3,3,3,3,3,3,3,3,3,3,3,3,3,3,3,3,3,3,3,3,3,3,3,3,3,3,3,3,3,
3,3,3,4),(-74.4041946699734,-74.2989154700527,-74.1907886322468,-74.0851817966569,
-73.9757949577429,-73.8664081188289,-73.7640406558711,-73.6618235857204,
-73.5597261017602,-73.4576934119709,-73.3556925036279,-73.2536904063192,
-73.1515839955417,-73.0494242509036,-72.9470820091423,-72.8682134145204,
-72.7658463531009,-72.6636296930376,-72.5615326300271,-72.4595003676406,
-72.3574998925447,-72.2554982337247,-72.1533922665579,-72.0512329690712,
-71.9488911752294,-71.8700187102119,-71.7676513447524,-71.665434376083,
-71.5633369991085,-71.4613044196293,-71.3593036247673,-71.2573016439608,
-71.1551953535957,-71.0530357317292,-70.9506936152493,-70.8718240059034,
-70.7694567046396,-70.6672398004949,-70.565142488222,-70.4631099735199,
-70.3611092434162,-70.2591073272548,-70.1570011009025,-70.0548415427991,
-69.9524994889408,-69.8736293015949,-69.7712620420592,-69.6690451806148,
-69.566947912297,-69.4649154422974,-69.3629147575807,-69.2609128874278,
-69.1588067077335,-69.056647196722,-68.9543051901375,-68.8754345972864,
-68.7743268238781,-68.6733543158174,-68.5724823531886,-68.4716763501524,
-68.3708710416405,-68.2700671456386,-68.1691815073704,-68.1210093627937),
 .UNSPECIFIED.);
#1200=B_SPLINE_CURVE_WITH_KNOTS('',3,(#12170,#12171,#12172,#12173,#12174,
#12175,#12176,#12177,#12178,#12179,#12180,#12181,#12182,#12183,#12184,#12185,
#12186,#12187,#12188,#12189,#12190,#12191,#12192,#12193,#12194,#12195,#12196,
#12197,#12198,#12199,#12200,#12201,#12202,#12203,#12204,#12205,#12206,#12207,
#12208,#12209,#12210,#12211,#12212,#12213,#12214,#12215,#12216,#12217,#12218,
#12219,#12220,#12221,#12222,#12223,#12224,#12225,#12226,#12227,#12228,#12229,
#12230,#12231,#12232,#12233,#12234,#12235,#12236,#12237,#12238,#12239,#12240,
#12241,#12242,#12243,#12244,#12245,#12246,#12247,#12248,#12249,#12250,#12251,
#12252,#12253,#12254,#12255,#12256,#12257,#12258,#12259,#12260,#12261,#12262,
#12263,#12264,#12265,#12266,#12267,#12268,#12269,#12270,#12271,#12272,#12273,
#12274,#12275,#12276,#12277,#12278,#12279,#12280,#12281,#12282,#12283,#12284,
#12285,#12286,#12287,#12288,#12289,#12290,#12291,#12292,#12293,#12294,#12295,
#12296,#12297,#12298,#12299,#12300,#12301,#12302,#12303,#12304,#12305,#12306,
#12307,#12308,#12309,#12310,#12311,#12312,#12313,#12314,#12315,#12316,#12317,
#12318,#12319,#12320,#12321,#12322,#12323,#12324,#12325,#12326,#12327,#12328,
#12329,#12330,#12331,#12332,#12333,#12334,#12335,#12336,#12337,#12338,#12339,
#12340,#12341,#12342,#12343,#12344,#12345,#12346,#12347,#12348,#12349,#12350,
#12351,#12352,#12353,#12354,#12355,#12356,#12357,#12358,#12359),
 .UNSPECIFIED.,.F.,.F.,(4,3,3,3,3,3,3,3,3,3,3,3,3,3,3,3,3,3,3,3,3,3,3,3,
3,3,3,3,3,3,3,3,3,3,3,3,3,3,3,3,3,3,3,3,3,3,3,3,3,3,3,3,3,3,3,3,3,3,3,3,
3,3,3,4),(-68.1210093625646,-67.9871254872857,-67.8772398929779,-67.7748726051917,
-67.6726557149727,-67.5705584172322,-67.4685259174276,-67.3665252025655,
-67.2645233019694,-67.1624170915797,-67.0602575496844,-66.9579155122564,
-66.8790451886694,-66.7766779048991,-66.6744610188026,-66.5723637253247,
-66.4703312298665,-66.3683305194287,-66.2663286233285,-66.1642224175153,
-66.0620628802484,-65.959720847482,-65.8808504843609,-65.7784831957226,
-65.676266304678,-65.5741690061558,-65.4721365055967,-65.3701357900088,
-65.2681338887165,-65.166027677682,-65.0638681351694,-64.9615260971768,
-64.8826557800524,-64.7802884930504,-64.6780716036587,-64.5759743068065,
-64.4739418079271,-64.371941094026,-64.2699391944252,-64.1678329850779,
-64.0656734442527,-63.9633314079284,-63.8844610757439,-63.7820937890789,
-63.6798769000354,-63.5777796035463,-63.4757471050391,-63.3737463915186,
-63.2717444923066,-63.1696382833577,-63.067478742937,-62.9651367070226,
-62.8862663714354,-62.7838990841745,-62.6816821945248,-62.579584897417,
-62.4775523982838,-62.3755516841309,-62.2735497842809,-62.1714435746897,
-62.0692840336235,-61.9669419970654,-61.8880716671269,-61.8378240556142),
 .UNSPECIFIED.);
#1201=B_SPLINE_CURVE_WITH_KNOTS('',3,(#12361,#12362,#12363,#12364,#12365,
#12366,#12367,#12368,#12369,#12370,#12371,#12372,#12373,#12374,#12375,#12376,
#12377,#12378,#12379,#12380,#12381,#12382,#12383,#12384,#12385,#12386,#12387,
#12388,#12389,#12390,#12391,#12392,#12393,#12394,#12395,#12396,#12397,#12398,
#12399,#12400,#12401,#12402,#12403,#12404,#12405,#12406,#12407,#12408,#12409,
#12410,#12411,#12412,#12413,#12414,#12415,#12416,#12417,#12418,#12419,#12420,
#12421,#12422,#12423,#12424,#12425,#12426,#12427,#12428,#12429,#12430,#12431,
#12432,#12433,#12434,#12435,#12436,#12437,#12438,#12439,#12440,#12441,#12442,
#12443,#12444,#12445,#12446,#12447,#12448,#12449,#12450,#12451,#12452,#12453,
#12454,#12455,#12456,#12457,#12458,#12459,#12460,#12461,#12462,#12463,#12464,
#12465,#12466,#12467,#12468,#12469,#12470,#12471,#12472,#12473,#12474,#12475,
#12476,#12477,#12478,#12479,#12480,#12481,#12482,#12483,#12484,#12485,#12486,
#12487,#12488,#12489,#12490,#12491,#12492,#12493,#12494,#12495,#12496,#12497,
#12498,#12499,#12500,#12501,#12502,#12503,#12504,#12505,#12506,#12507,#12508,
#12509,#12510,#12511,#12512,#12513,#12514,#12515,#12516,#12517,#12518,#12519,
#12520,#12521,#12522,#12523,#12524,#12525,#12526,#12527,#12528,#12529,#12530,
#12531,#12532,#12533,#12534,#12535,#12536,#12537,#12538,#12539,#12540,#12541,
#12542,#12543,#12544,#12545,#12546,#12547,#12548,#12549,#12550),
 .UNSPECIFIED.,.F.,.F.,(4,3,3,3,3,3,3,3,3,3,3,3,3,3,3,3,3,3,3,3,3,3,3,3,
3,3,3,3,3,3,3,3,3,3,3,3,3,3,3,3,3,3,3,3,3,3,3,3,3,3,3,3,3,3,3,3,3,3,3,3,
3,3,3,4),(-61.8378240552875,-61.7362592426383,-61.6304614576608,-61.5291566919834,
-61.4279088057521,-61.3266837808246,-61.2254476335928,-61.1241031222742,
-61.0226944346116,-60.9211196171127,-60.8898769628184,-60.7875096758169,
-60.6852927864304,-60.5831954895903,-60.4811629907274,-60.379162276847,
-60.2771603772715,-60.1750541679557,-60.0728946271658,-59.9705525908826,
-59.8916822585099,-59.7893149714371,-59.6870980819781,-59.585000785064,
-59.4829682861259,-59.3809675721698,-59.2789656725175,-59.1768594631247,
-59.0746999222572,-58.9723578858965,-58.8934875542014,-58.7911202671623,
-58.6889033777374,-58.5868060808579,-58.4847735819549,-58.3827728680338,
-58.2807709684166,-58.178664759059,-58.076505218227,-57.9741631819014,-57.8952928498929,
-57.7929255628534,-57.6907086734283,-57.5886113765486,-57.4865788776455,
-57.3845781637245,-57.2825762641079,-57.1804700547506,-57.078310513919,
-56.9759684775939,-56.8970981455844,-56.7947308585367,-56.6925139691031,
-56.5904166722148,-56.488384173303,-56.3863834593731,-56.284381559747,-56.1822753503807,
-56.0801158095398,-55.9777737732056,-55.8989034412759,-55.7799885722811,
-55.66215376343,-55.5546387488805),.UNSPECIFIED.);
#1202=B_SPLINE_CURVE_WITH_KNOTS('',3,(#12552,#12553,#12554,#12555,#12556,
#12557,#12558,#12559,#12560,#12561,#12562,#12563,#12564,#12565,#12566,#12567,
#12568,#12569,#12570,#12571,#12572,#12573,#12574,#12575,#12576,#12577,#12578,
#12579,#12580,#12581,#12582,#12583,#12584,#12585,#12586,#12587,#12588,#12589,
#12590,#12591,#12592,#12593,#12594,#12595,#12596,#12597,#12598,#12599,#12600,
#12601,#12602,#12603,#12604,#12605,#12606,#12607,#12608,#12609,#12610,#12611,
#12612,#12613,#12614,#12615,#12616,#12617,#12618,#12619,#12620,#12621,#12622,
#12623,#12624,#12625,#12626,#12627,#12628,#12629,#12630,#12631,#12632,#12633,
#12634,#12635,#12636,#12637,#12638,#12639,#12640,#12641,#12642,#12643,#12644,
#12645,#12646,#12647,#12648,#12649,#12650,#12651,#12652,#12653,#12654,#12655,
#12656,#12657,#12658,#12659,#12660,#12661,#12662,#12663,#12664,#12665,#12666,
#12667,#12668,#12669,#12670,#12671,#12672,#12673,#12674,#12675,#12676,#12677,
#12678,#12679,#12680,#12681,#12682,#12683,#12684,#12685,#12686,#12687,#12688,
#12689,#12690,#12691,#12692,#12693,#12694,#12695,#12696,#12697,#12698,#12699,
#12700,#12701,#12702,#12703,#12704,#12705,#12706,#12707,#12708,#12709,#12710,
#12711,#12712,#12713,#12714,#12715,#12716,#12717,#12718,#12719,#12720,#12721,
#12722,#12723,#12724,#12725,#12726,#12727,#12728,#12729,#12730,#12731,#12732,
#12733,#12734,#12735,#12736,#12737,#12738,#12739,#12740,#12741,#12742,#12743,
#12744),.UNSPECIFIED.,.F.,.F.,(4,3,3,3,3,3,3,3,3,3,3,3,3,3,3,3,3,3,3,3,
3,3,3,3,3,3,3,3,3,3,3,3,3,3,3,3,3,3,3,3,3,3,3,3,3,3,3,3,3,3,3,3,3,3,3,3,
3,3,3,3,3,3,3,3,4),(-55.5546387484345,-55.4524945919236,-55.3503595415392,
-55.2482010148576,-55.145916884721,-55.0435604152556,-54.9410225331627,
-54.9007087369674,-54.7983414499237,-54.6961245604944,-54.5940272636104,
-54.491994764703,-54.3899940507776,-54.2879921511563,-54.1858859417944,
-54.0837264009581,-53.9813843646284,-53.9025140326589,-53.8001467456144,
-53.697929856184,-53.595832559299,-53.4938000603905,-53.391799346464,-53.2897974468418,
-53.1876912374789,-53.0855316966414,-52.9831896603107,-52.9043193283504,
-52.8019520413066,-52.6997351518768,-52.5976378549925,-52.4956053560847,
-52.3936046421589,-52.2916027425373,-52.189496533175,-52.0873369923383,
-51.9849949560081,-51.9061246240419,-51.803757336998,-51.7015404475684,
-51.599443150684,-51.4974106517761,-51.3954099378501,-51.2934080382284,
-51.1913018288661,-51.0891422880293,-50.9868002516991,-50.9079299197334,
-50.8055626326894,-50.7033457432593,-50.6012484463748,-50.4992159474668,
-50.397215233541,-50.295213333919,-50.1931071245565,-50.0909475837196,-49.9886055473893,
-49.9097352154249,-49.8068704917154,-49.7041587195511,-49.6015675718968,
-49.499067717916,-49.3966196681602,-49.2941789169835,-49.271453441255),
 .UNSPECIFIED.);
#1203=B_SPLINE_CURVE_WITH_KNOTS('',3,(#12746,#12747,#12748,#12749,#12750,
#12751,#12752,#12753,#12754,#12755,#12756,#12757,#12758,#12759,#12760,#12761,
#12762,#12763,#12764,#12765,#12766,#12767,#12768,#12769,#12770,#12771,#12772,
#12773,#12774,#12775,#12776,#12777,#12778,#12779,#12780,#12781,#12782,#12783,
#12784,#12785,#12786,#12787,#12788,#12789,#12790,#12791,#12792,#12793,#12794,
#12795,#12796,#12797,#12798,#12799,#12800,#12801,#12802,#12803,#12804,#12805,
#12806,#12807,#12808,#12809,#12810,#12811,#12812,#12813,#12814,#12815,#12816,
#12817,#12818,#12819,#12820,#12821,#12822,#12823,#12824,#12825,#12826,#12827,
#12828,#12829,#12830,#12831,#12832,#12833,#12834,#12835,#12836,#12837,#12838,
#12839,#12840,#12841,#12842,#12843,#12844,#12845,#12846,#12847,#12848,#12849,
#12850,#12851,#12852,#12853,#12854,#12855,#12856,#12857,#12858,#12859,#12860,
#12861,#12862,#12863,#12864,#12865,#12866,#12867,#12868,#12869,#12870,#12871,
#12872,#12873,#12874,#12875,#12876,#12877,#12878,#12879,#12880,#12881,#12882,
#12883,#12884,#12885,#12886,#12887,#12888,#12889,#12890,#12891,#12892,#12893,
#12894,#12895,#12896,#12897,#12898,#12899,#12900,#12901,#12902,#12903,#12904,
#12905,#12906,#12907,#12908,#12909,#12910,#12911,#12912,#12913,#12914,#12915,
#12916,#12917,#12918,#12919,#12920,#12921,#12922,#12923,#12924,#12925,#12926,
#12927,#12928,#12929,#12930,#12931,#12932,#12933,#12934,#12935),
 .UNSPECIFIED.,.F.,.F.,(4,3,3,3,3,3,3,3,3,3,3,3,3,3,3,3,3,3,3,3,3,3,3,3,
3,3,3,3,3,3,3,3,3,3,3,3,3,3,3,3,3,3,3,3,3,3,3,3,3,3,3,3,3,3,3,3,3,3,3,3,
3,3,3,4),(-49.2714534410242,-49.1553637467566,-49.0334521289365,-48.9115405111164,
-48.8091732240723,-48.7069563346426,-48.6048590377581,-48.5028265388501,
-48.4008258249242,-48.2988239253026,-48.1967177159402,-48.0945581751034,
-47.9922161387732,-47.9133458068079,-47.8109785197638,-47.7087616303339,
-47.6066643334494,-47.5046318345414,-47.4026311206155,-47.3006292209937,
-47.1985230116313,-47.0963634707945,-46.9940214344642,-46.9151511024994,
-46.8127838154554,-46.7105669260255,-46.608469629141,-46.5064371302331,
-46.4044364163071,-46.3024345166853,-46.200328307323,-46.0981687664861,
-45.9958267301559,-45.9169563981909,-45.8145891111468,-45.712372221717,
-45.6102749248325,-45.5082424259245,-45.4062417119986,-45.3042398123768,
-45.2021336030144,-45.0999740621776,-44.9976320258473,-44.9187616938824,
-44.8163944068383,-44.7141775174084,-44.612080220524,-44.510047721616,-44.40804700769,
-44.3060451080683,-44.2039388987059,-44.101779357869,-43.9994373215388,
-43.9205669895739,-43.8191696623787,-43.7153069713905,-43.6141779904582,
-43.5131096780641,-43.4120678056774,-43.3061178878761,-43.2049654936796,
-43.1037498433122,-43.0023807665007,-42.9882681344725),.UNSPECIFIED.);
#1204=B_SPLINE_CURVE_WITH_KNOTS('',3,(#12937,#12938,#12939,#12940,#12941,
#12942,#12943,#12944,#12945,#12946,#12947,#12948,#12949,#12950,#12951,#12952,
#12953,#12954,#12955,#12956,#12957,#12958,#12959,#12960,#12961,#12962,#12963,
#12964,#12965,#12966,#12967,#12968,#12969,#12970,#12971,#12972,#12973,#12974,
#12975,#12976,#12977,#12978,#12979,#12980,#12981,#12982,#12983,#12984,#12985,
#12986,#12987,#12988,#12989,#12990,#12991,#12992,#12993,#12994,#12995,#12996,
#12997,#12998,#12999,#13000,#13001,#13002,#13003,#13004,#13005,#13006,#13007,
#13008,#13009,#13010,#13011,#13012,#13013,#13014,#13015,#13016,#13017,#13018,
#13019,#13020,#13021,#13022,#13023,#13024,#13025,#13026,#13027,#13028,#13029,
#13030,#13031,#13032,#13033,#13034,#13035,#13036,#13037,#13038,#13039,#13040,
#13041,#13042,#13043,#13044,#13045,#13046,#13047,#13048,#13049,#13050,#13051,
#13052,#13053,#13054,#13055,#13056,#13057,#13058,#13059,#13060,#13061,#13062,
#13063,#13064,#13065,#13066,#13067,#13068,#13069,#13070,#13071,#13072,#13073,
#13074,#13075,#13076,#13077,#13078,#13079,#13080,#13081,#13082,#13083,#13084,
#13085,#13086,#13087,#13088,#13089,#13090,#13091,#13092,#13093,#13094,#13095,
#13096,#13097,#13098,#13099,#13100,#13101,#13102,#13103,#13104,#13105,#13106,
#13107,#13108,#13109,#13110,#13111,#13112,#13113,#13114,#13115,#13116,#13117,
#13118,#13119,#13120,#13121,#13122,#13123,#13124,#13125,#13126),
 .UNSPECIFIED.,.F.,.F.,(4,3,3,3,3,3,3,3,3,3,3,3,3,3,3,3,3,3,3,3,3,3,3,3,
3,3,3,3,3,3,3,3,3,3,3,3,3,3,3,3,3,3,3,3,3,3,3,3,3,3,3,3,3,3,3,3,3,3,3,3,
3,3,3,4),(-42.9882681340755,-42.9223722852654,-42.8200049982217,-42.7177881087921,
-42.615690811908,-42.5136583130004,-42.4116575990748,-42.3096556994534,
-42.2075494900914,-42.105389949255,-42.0030479129251,-41.9241775809569,
-41.8218102939128,-41.719593404483,-41.6174961075985,-41.5154636086904,
-41.4134628947644,-41.3114609951426,-41.2093547857802,-41.1071952449433,
-41.004853208613,-40.9259828766484,-40.8236155896043,-40.7213987001744,
-40.61930140329,-40.517268904382,-40.415268190456,-40.3132662908342,-40.2111600814718,
-40.1090005406349,-40.0066585043046,-39.92778817234,-39.825420885296,-39.7232039958661,
-39.6211066989817,-39.5190742000737,-39.4170734861478,-39.315071586526,
-39.2129653771637,-39.1108058363269,-39.0084637999966,-38.9295934680314,
-38.8272261809873,-38.7250092915574,-38.622911994673,-38.5208794957649,
-38.4188787818389,-38.316876882217,-38.2147706728546,-38.1126111320177,
-38.0102690956874,-37.9313987637229,-37.8290314766789,-37.726814587249,
-37.6247172903646,-37.5226847914566,-37.4206840775307,-37.318682177909,
-37.2165759685467,-37.1144164277098,-37.0120743913795,-36.9332040594144,
-36.7954612711504,-36.7050828268958),.UNSPECIFIED.);
#1205=B_SPLINE_CURVE_WITH_KNOTS('',3,(#13128,#13129,#13130,#13131,#13132,
#13133,#13134,#13135,#13136,#13137,#13138,#13139,#13140,#13141,#13142,#13143,
#13144,#13145,#13146,#13147,#13148,#13149,#13150,#13151,#13152,#13153,#13154,
#13155,#13156,#13157,#13158,#13159,#13160,#13161,#13162,#13163,#13164,#13165,
#13166,#13167,#13168,#13169,#13170,#13171,#13172,#13173,#13174,#13175,#13176,
#13177,#13178,#13179,#13180,#13181,#13182,#13183,#13184,#13185,#13186,#13187,
#13188,#13189,#13190,#13191,#13192,#13193,#13194,#13195,#13196,#13197,#13198,
#13199,#13200,#13201,#13202,#13203,#13204,#13205,#13206,#13207,#13208,#13209,
#13210,#13211,#13212,#13213,#13214,#13215,#13216,#13217,#13218,#13219,#13220,
#13221,#13222,#13223,#13224,#13225,#13226,#13227,#13228,#13229,#13230,#13231,
#13232,#13233,#13234,#13235,#13236,#13237,#13238,#13239,#13240,#13241,#13242,
#13243,#13244,#13245,#13246,#13247,#13248,#13249,#13250,#13251,#13252,#13253,
#13254,#13255,#13256,#13257,#13258,#13259,#13260,#13261,#13262,#13263,#13264,
#13265,#13266,#13267,#13268,#13269,#13270,#13271,#13272,#13273,#13274,#13275,
#13276,#13277,#13278,#13279,#13280,#13281,#13282,#13283,#13284,#13285,#13286,
#13287,#13288,#13289,#13290,#13291,#13292,#13293,#13294,#13295,#13296,#13297,
#13298,#13299,#13300,#13301,#13302,#13303,#13304,#13305,#13306,#13307,#13308,
#13309,#13310,#13311,#13312,#13313,#13314,#13315,#13316,#13317),
 .UNSPECIFIED.,.F.,.F.,(4,3,3,3,3,3,3,3,3,3,3,3,3,3,3,3,3,3,3,3,3,3,3,3,
3,3,3,3,3,3,3,3,3,3,3,3,3,3,3,3,3,3,3,3,3,3,3,3,3,3,3,3,3,3,3,3,3,3,3,3,
3,3,3,4),(-36.7050828266525,-36.6042885945794,-36.5035674624096,-36.4028848059392,
-36.3022060553303,-36.2014299820177,-36.1006021640577,-35.999600330535,
-35.9350093551059,-35.8326420680619,-35.7304251786319,-35.6283278817475,
-35.5262953828395,-35.4242946689136,-35.3222927692918,-35.2201865599295,
-35.1180270190926,-35.0156849827623,-34.9368146507975,-34.8344473637536,
-34.7322304743239,-34.6301331774395,-34.5281006785315,-34.4260999646055,
-34.3240980649836,-34.2219918556213,-34.1198323147845,-34.0174902784543,
-33.9386199464889,-33.836252659445,-33.7340357700152,-33.6319384731309,
-33.5299059742231,-33.4279052602974,-33.3259033606756,-33.2237971513134,
-33.1216376104767,-33.0192955741466,-32.9404252421805,-32.838057955136,
-32.7358410657059,-32.633743768821,-32.5317112699125,-32.429710555986,-32.3277086563638,
-32.225602447001,-32.1234429061638,-32.0211008698331,-31.942230537872,-31.8398632508286,
-31.7376463613988,-31.6355490645148,-31.5335165656073,-31.4315158516818,
-31.3295139520605,-31.2274077426987,-31.1252482018621,-31.0229061655323,
-30.9440358335635,-30.8374542773428,-30.7311507425934,-30.6250112048688,
-30.5190642728785,-30.4218975197163),.UNSPECIFIED.);
#1206=B_SPLINE_CURVE_WITH_KNOTS('',3,(#13319,#13320,#13321,#13322,#13323,
#13324,#13325,#13326,#13327,#13328,#13329,#13330,#13331,#13332,#13333,#13334,
#13335,#13336,#13337,#13338,#13339,#13340,#13341,#13342,#13343,#13344,#13345,
#13346,#13347,#13348,#13349,#13350,#13351,#13352,#13353,#13354,#13355,#13356,
#13357,#13358,#13359,#13360,#13361,#13362,#13363,#13364,#13365,#13366,#13367,
#13368,#13369,#13370,#13371,#13372,#13373,#13374,#13375,#13376,#13377,#13378,
#13379,#13380,#13381,#13382,#13383,#13384,#13385,#13386,#13387,#13388,#13389,
#13390,#13391,#13392,#13393,#13394,#13395,#13396,#13397,#13398,#13399,#13400,
#13401,#13402,#13403,#13404,#13405,#13406,#13407,#13408,#13409,#13410,#13411,
#13412,#13413,#13414,#13415,#13416,#13417,#13418,#13419,#13420,#13421,#13422,
#13423,#13424,#13425,#13426,#13427,#13428,#13429,#13430,#13431,#13432,#13433,
#13434,#13435,#13436,#13437,#13438,#13439,#13440,#13441,#13442,#13443,#13444,
#13445,#13446,#13447,#13448,#13449,#13450,#13451,#13452,#13453,#13454,#13455,
#13456,#13457,#13458,#13459,#13460,#13461,#13462,#13463,#13464,#13465,#13466,
#13467,#13468,#13469,#13470,#13471,#13472,#13473,#13474,#13475,#13476,#13477,
#13478,#13479,#13480,#13481,#13482,#13483,#13484,#13485,#13486,#13487,#13488,
#13489,#13490,#13491,#13492,#13493,#13494,#13495,#13496,#13497,#13498,#13499,
#13500,#13501,#13502,#13503,#13504,#13505,#13506,#13507,#13508),
 .UNSPECIFIED.,.F.,.F.,(4,3,3,3,3,3,3,3,3,3,3,3,3,3,3,3,3,3,3,3,3,3,3,3,
3,3,3,3,3,3,3,3,3,3,3,3,3,3,3,3,3,3,3,3,3,3,3,3,3,3,3,3,3,3,3,3,3,3,3,3,
3,3,3,4),(-30.4218975194729,-30.3139822064023,-30.2057128646672,-30.0972539529647,
-29.98848589277,-29.945841129255,-29.843473842207,-29.7412569527731,-29.6391596558847,
-29.5371271569728,-29.4351264430428,-29.333124543417,-29.2310183340508,
-29.12885879321,-29.026516756876,-28.9476464249465,-28.8452791379076,-28.7430622484828,
-28.6409649516034,-28.5389324527004,-28.4369317387794,-28.3349298391625,
-28.2328236298049,-28.1306640889728,-28.0283220526472,-27.949451720638,
-27.8470844335986,-27.7448675441735,-27.6427702472938,-27.5407377483907,
-27.4387370344697,-27.3367351348528,-27.2346289254954,-27.1324693846636,
-27.0301273483383,-26.9512570163295,-26.8488897292551,-26.7466728397948,
-26.64457554288,-26.5425430439417,-26.4405423299855,-26.3385404303335,-26.2364342209414,
-26.134274680075,-26.0319326437158,-25.953062312021,-25.8506950250239,-25.7484781356409,
-25.6463808388029,-25.5443483399411,-25.442347626061,-25.3403457264847,
-25.2382395171668,-25.136079976374,-25.0337379400866,-24.9548676077125,
-24.8528481833478,-24.7521697733989,-24.6515876604174,-24.5510669891891,
-24.4479782950907,-24.347434160888,-24.2430731868416,-24.1387122127952),
 .UNSPECIFIED.);
#1207=B_SPLINE_CURVE_WITH_KNOTS('',3,(#13510,#13511,#13512,#13513,#13514,
#13515,#13516,#13517,#13518,#13519,#13520,#13521,#13522,#13523,#13524,#13525,
#13526,#13527,#13528,#13529,#13530,#13531,#13532,#13533,#13534,#13535,#13536,
#13537,#13538,#13539,#13540,#13541,#13542,#13543,#13544,#13545,#13546,#13547,
#13548,#13549,#13550,#13551,#13552,#13553,#13554,#13555,#13556,#13557,#13558,
#13559,#13560,#13561,#13562,#13563,#13564,#13565,#13566,#13567,#13568,#13569,
#13570,#13571,#13572,#13573,#13574,#13575,#13576,#13577,#13578,#13579,#13580,
#13581,#13582,#13583,#13584,#13585,#13586,#13587,#13588,#13589,#13590,#13591,
#13592,#13593,#13594,#13595,#13596,#13597,#13598,#13599,#13600,#13601,#13602,
#13603,#13604,#13605,#13606,#13607,#13608,#13609,#13610,#13611,#13612,#13613,
#13614,#13615,#13616,#13617,#13618,#13619,#13620,#13621,#13622,#13623,#13624,
#13625,#13626,#13627,#13628,#13629,#13630,#13631,#13632,#13633,#13634,#13635,
#13636,#13637,#13638,#13639,#13640,#13641,#13642,#13643,#13644,#13645,#13646,
#13647,#13648,#13649,#13650,#13651,#13652,#13653,#13654,#13655,#13656,#13657,
#13658,#13659,#13660,#13661,#13662,#13663,#13664,#13665,#13666,#13667,#13668,
#13669,#13670,#13671,#13672,#13673,#13674,#13675,#13676,#13677,#13678,#13679,
#13680,#13681,#13682,#13683,#13684,#13685,#13686,#13687,#13688,#13689,#13690,
#13691,#13692,#13693,#13694,#13695,#13696,#13697,#13698,#13699),
 .UNSPECIFIED.,.F.,.F.,(4,3,3,3,3,3,3,3,3,3,3,3,3,3,3,3,3,3,3,3,3,3,3,3,
3,3,3,3,3,3,3,3,3,3,3,3,3,3,3,3,3,3,3,3,3,3,3,3,3,3,3,3,3,3,3,3,3,3,3,3,
3,3,3,4),(-24.1387122125366,-23.9846718531693,-23.956672903404,-23.8543056161328,
-23.752088726475,-23.6499914293626,-23.5479589302269,-23.4459582160735,
-23.343956316225,-23.2418501066388,-23.1396905655791,-23.0373485290305,
-22.9584781990955,-22.8561109124667,-22.7538940234513,-22.6517967269784,
-22.5497642284799,-22.4477635149608,-22.3457616157428,-22.2436554067765,
-22.1414958663321,-22.0391538303839,-21.960283494787,-21.8579162077476,
-21.7556993183269,-21.653602021458,-21.5515695225696,-21.4495688086671,
-21.3475669090727,-21.2454606997433,-21.1433011589426,-21.0409591226533,
-20.9620887904785,-20.8597215017776,-20.7575046106841,-20.6554073121339,
-20.5533748115597,-20.4513740959694,-20.3493721946875,-20.247265983683,
-20.1451064412114,-20.0427644032773,-19.96389408617,-19.8615268026831,-19.7593099168074,
-19.6572126234559,-19.5551801280662,-19.4531794176392,-19.3511775214919,
-19.2490713155426,-19.14691177809,-19.0445697450586,-18.9656993818615,-18.8633320937121,
-18.7611152032101,-18.6590179053077,-18.5569854054153,-18.4549846905396,
-18.352982790004,-18.2508765797888,-18.1487170381317,-18.0463750010433,
-17.967504677553,-17.8555269053571),.UNSPECIFIED.);
#1208=B_SPLINE_CURVE_WITH_KNOTS('',3,(#13701,#13702,#13703,#13704,#13705,
#13706,#13707,#13708,#13709,#13710,#13711,#13712,#13713,#13714,#13715,#13716,
#13717,#13718,#13719,#13720,#13721,#13722,#13723,#13724,#13725,#13726,#13727,
#13728,#13729,#13730,#13731,#13732,#13733,#13734,#13735,#13736,#13737,#13738,
#13739,#13740,#13741,#13742,#13743,#13744,#13745,#13746,#13747,#13748,#13749,
#13750,#13751,#13752,#13753,#13754,#13755,#13756,#13757,#13758,#13759,#13760,
#13761,#13762,#13763,#13764,#13765,#13766,#13767,#13768,#13769,#13770,#13771,
#13772,#13773,#13774,#13775,#13776,#13777,#13778,#13779,#13780,#13781,#13782,
#13783,#13784,#13785,#13786,#13787,#13788,#13789,#13790,#13791,#13792,#13793,
#13794,#13795,#13796,#13797,#13798,#13799,#13800,#13801,#13802,#13803,#13804,
#13805,#13806,#13807,#13808,#13809,#13810,#13811,#13812,#13813,#13814,#13815,
#13816,#13817,#13818,#13819,#13820,#13821,#13822,#13823,#13824,#13825,#13826,
#13827,#13828,#13829,#13830,#13831,#13832,#13833,#13834,#13835,#13836,#13837,
#13838,#13839,#13840,#13841,#13842,#13843,#13844,#13845,#13846,#13847,#13848,
#13849,#13850,#13851,#13852,#13853,#13854,#13855,#13856,#13857,#13858,#13859,
#13860,#13861,#13862,#13863,#13864,#13865,#13866,#13867,#13868,#13869,#13870,
#13871,#13872,#13873,#13874,#13875,#13876,#13877,#13878,#13879,#13880,#13881,
#13882,#13883,#13884,#13885,#13886,#13887,#13888,#13889,#13890),
 .UNSPECIFIED.,.F.,.F.,(4,3,3,3,3,3,3,3,3,3,3,3,3,3,3,3,3,3,3,3,3,3,3,3,
3,3,3,3,3,3,3,3,3,3,3,3,3,3,3,3,3,3,3,3,3,3,3,3,3,3,3,3,3,3,3,3,3,3,3,3,
3,3,3,4),(-17.8555269049038,-17.7545911196499,-17.6537987523961,-17.5530852258919,
-17.4524158822442,-17.3517561249875,-17.2510031448081,-17.1502034731529,
-17.0492255787679,-16.9693099732445,-16.8669427158835,-16.7647258561339,
-16.6626285887859,-16.5605961193123,-16.458595434678,-16.3565935641645,
-16.2544873834259,-16.1523278709894,-16.0499858623717,-15.971115268936,
-15.868747964328,-15.7665310575775,-15.664433743813,-15.5624012283022,-15.4604004980717,
-15.3583985824649,-15.2562923577183,-15.1541328018062,-15.0517907510743,
-14.9729205646275,-14.8705531977598,-14.7683362279927,-14.6662388503901,
-14.5642062705704,-14.4622054756551,-14.3602034950823,-14.2580972053933,
-14.1559375844495,-14.0535954692861,-13.974725860319,-13.8723588152025,
-13.7701421678431,-13.6680451121038,-13.5660128536591,-13.4640123791809,
-13.3620107176574,-13.2599047426625,-13.1577454344935,-13.0554036254108,
-12.9765311560105,-12.8741636634534,-12.7719465702381,-12.6698490730764,
-12.5678163761306,-12.4658154666658,-12.3638133742659,-12.261706977701,
-12.1595472524578,-12.057205038368,-11.978336451702,-11.865143194293,-11.7522969553209,
-11.6400318303335,-11.572341598581),.UNSPECIFIED.);
#1209=B_SPLINE_CURVE_WITH_KNOTS('',3,(#13892,#13893,#13894,#13895,#13896,
#13897,#13898,#13899,#13900,#13901,#13902,#13903,#13904,#13905,#13906,#13907,
#13908,#13909,#13910,#13911,#13912,#13913,#13914,#13915,#13916,#13917,#13918,
#13919,#13920,#13921,#13922,#13923,#13924,#13925,#13926,#13927,#13928,#13929,
#13930,#13931,#13932,#13933,#13934,#13935,#13936,#13937,#13938,#13939,#13940,
#13941,#13942,#13943,#13944,#13945,#13946,#13947,#13948,#13949,#13950,#13951,
#13952,#13953,#13954,#13955,#13956,#13957,#13958,#13959,#13960,#13961,#13962,
#13963,#13964,#13965,#13966,#13967,#13968,#13969,#13970,#13971,#13972,#13973,
#13974,#13975,#13976,#13977,#13978,#13979,#13980,#13981,#13982,#13983,#13984,
#13985,#13986,#13987,#13988,#13989,#13990,#13991,#13992,#13993,#13994,#13995,
#13996,#13997,#13998,#13999,#14000,#14001,#14002,#14003,#14004,#14005,#14006,
#14007,#14008,#14009,#14010,#14011,#14012,#14013,#14014,#14015,#14016,#14017,
#14018,#14019,#14020,#14021,#14022,#14023,#14024,#14025,#14026,#14027,#14028,
#14029,#14030,#14031,#14032,#14033,#14034,#14035,#14036,#14037,#14038,#14039,
#14040,#14041,#14042,#14043,#14044,#14045,#14046,#14047,#14048,#14049,#14050,
#14051,#14052,#14053,#14054,#14055,#14056,#14057,#14058,#14059,#14060,#14061,
#14062,#14063,#14064,#14065,#14066,#14067,#14068,#14069,#14070,#14071,#14072,
#14073,#14074,#14075,#14076,#14077,#14078,#14079,#14080,#14081),
 .UNSPECIFIED.,.F.,.F.,(4,3,3,3,3,3,3,3,3,3,3,3,3,3,3,3,3,3,3,3,3,3,3,3,
3,3,3,3,3,3,3,3,3,3,3,3,3,3,3,3,3,3,3,3,3,3,3,3,3,3,3,3,3,3,3,3,3,3,3,3,
3,3,3,4),(-11.5723415981774,-11.4687871680508,-11.3651903770408,-11.2614377882717,
-11.1576027709896,-11.0535531293269,-10.9801417473935,-10.8777763889726,
-10.7755614305822,-10.6734660592423,-10.5714354815914,-10.4694366819606,
-10.3674366869917,-10.2653323542086,-10.1631746773412,-10.0608344631842,
-9.98194704308499,-9.87957764019733,-9.77735864674374,-9.67525927317135,
-9.57322471527629,-9.47122196281362,-9.36921804787462,-9.26710987283633,
-9.16494839075294,-9.06260447502326,-8.98375233877649,-8.88138196791595,
-8.77916195956028,-8.67706150654447,-8.57502583031432,-8.47302192255833,
-8.37101681726233,-8.26890740648803,-8.16674466156689,-8.06439945351,-7.98555763446799,
-7.88320538840778,-7.78100356872168,-7.67892131341409,-7.57690383165239,
-7.47491808949712,-7.37293109529183,-7.27083958565016,-7.1686946536896,
-7.06636691157338,-6.98736293015949,-6.88497539269428,-6.78273832980578,
-6.68062106799417,-6.57856874128089,-6.47654836352991,-6.374526991071,-6.27240173750569,
-6.17022336025357,-6.06786304006514,-5.98916822585099,-5.88745971193225,
-5.78589199605195,-5.68443102714422,-5.58302740004296,-5.4816616432721,
-5.38024993235094,-5.28915629099788),.UNSPECIFIED.);
#1210=B_SPLINE_CURVE_WITH_KNOTS('',3,(#14083,#14084,#14085,#14086,#14087,
#14088,#14089,#14090,#14091,#14092,#14093,#14094,#14095,#14096,#14097,#14098,
#14099,#14100,#14101,#14102,#14103,#14104,#14105,#14106,#14107,#14108,#14109,
#14110,#14111,#14112,#14113,#14114,#14115,#14116,#14117,#14118,#14119,#14120,
#14121,#14122,#14123,#14124,#14125,#14126,#14127,#14128,#14129,#14130,#14131,
#14132,#14133,#14134,#14135,#14136,#14137,#14138,#14139,#14140,#14141,#14142,
#14143,#14144,#14145,#14146,#14147,#14148,#14149,#14150,#14151,#14152,#14153,
#14154,#14155,#14156,#14157,#14158,#14159,#14160,#14161,#14162,#14163,#14164,
#14165,#14166,#14167,#14168,#14169,#14170,#14171,#14172,#14173,#14174,#14175,
#14176,#14177,#14178,#14179),.UNSPECIFIED.,.F.,.F.,(4,3,3,3,3,3,3,3,3,3,
3,3,3,3,3,3,3,3,3,3,3,3,3,3,3,3,3,3,3,3,3,3,4),(-5.2891562906822,-5.16592202403009,
-5.0409071101405,-4.99097352154249,-4.8887207823386,-4.78661873310371,-4.68463617498642,
-4.58271830049947,-4.48083193862712,-4.37894396049634,-4.27695022114797,
-4.17490252616154,-4.07267004030852,-3.99277881723399,-3.89022667007414,
-3.78782539108402,-3.68554527959923,-3.58333102513057,-3.48114986928111,
-3.37896909715953,-3.27668767666928,-3.17435468887112,-3.0718440432757,
-2.99458411292549,-2.89325038855348,-2.79021171641803,-2.68914057287426,
-2.58812832611143,-2.48714069765389,-2.38259077610789,-2.28148996903811,
-2.175215490254,-2.06894101146989),.UNSPECIFIED.);
#1211=B_SPLINE_CURVE_WITH_KNOTS('',3,(#14180,#14181,#14182,#14183),
 .UNSPECIFIED.,.F.,.F.,(4,4),(-0.0402655477269185,0.),.UNSPECIFIED.);
#1212=B_SPLINE_CURVE_WITH_KNOTS('',3,(#14186,#14187,#14188,#14189,#14190),
 .UNSPECIFIED.,.F.,.F.,(4,1,4),(95.7927227292494,96.5575686288105,97.3893656654685),
 .UNSPECIFIED.);
#1213=B_SPLINE_CURVE_WITH_KNOTS('',3,(#14192,#14193,#14194,#14195,#14196,
#14197,#14198,#14199,#14200,#14201,#14202,#14203,#14204,#14205,#14206,#14207,
#14208,#14209,#14210,#14211,#14212,#14213,#14214,#14215,#14216,#14217,#14218,
#14219,#14220,#14221,#14222,#14223,#14224,#14225,#14226,#14227,#14228,#14229,
#14230,#14231,#14232,#14233,#14234,#14235,#14236,#14237,#14238,#14239,#14240,
#14241,#14242,#14243,#14244,#14245,#14246,#14247,#14248,#14249,#14250,#14251,
#14252,#14253,#14254,#14255,#14256,#14257,#14258,#14259,#14260,#14261,#14262,
#14263,#14264,#14265,#14266,#14267,#14268,#14269,#14270,#14271,#14272,#14273,
#14274,#14275,#14276,#14277,#14278,#14279,#14280,#14281,#14282),
 .UNSPECIFIED.,.F.,.F.,(4,3,3,3,3,3,3,3,3,3,3,3,3,3,3,3,3,3,3,3,3,3,3,3,
3,3,3,3,3,3,4),(97.3893722612835,97.555763333119,97.6636833055627,97.7749676470458,
97.8825903472849,97.9901474011131,98.0976777951607,98.2052204718533,98.3128843396892,
98.4206214009902,98.5285425318896,98.5539580374275,98.6621940121476,98.7734388533462,
98.881375737639,98.9892454584003,99.0970865171573,99.2049373691907,99.3129038037117,
99.4209404931574,99.5291543370944,99.552152741736,99.6591027660594,99.7658697883256,
99.8725354114468,99.9791400170328,100.08572389744,100.192397532104,100.299117505247,
100.406021276585,100.477768433197),.UNSPECIFIED.);
#1214=B_SPLINE_CURVE_WITH_KNOTS('',3,(#14286,#14287,#14288,#14289,#14290,
#14291,#14292,#14293,#14294,#14295,#14296,#14297,#14298,#14299,#14300,#14301,
#14302,#14303,#14304,#14305,#14306,#14307,#14308,#14309,#14310,#14311,#14312,
#14313,#14314,#14315,#14316,#14317,#14318,#14319,#14320,#14321,#14322,#14323,
#14324,#14325,#14326,#14327,#14328,#14329,#14330,#14331,#14332,#14333,#14334,
#14335,#14336,#14337),.UNSPECIFIED.,.F.,.F.,(4,3,3,3,3,3,3,3,3,3,3,3,3,
3,3,3,3,4),(97.38937254813,97.4958016639887,97.6009101902419,97.7059494886238,
97.810961292752,97.9184223383138,98.0235759129497,98.1321906939746,98.2408054749994,
98.3517561547439,98.4626616578144,98.5732387102861,98.6837093999491,98.7941056372081,
98.9053292727331,99.0157026983767,99.1273514388423,99.2390001793079),
 .UNSPECIFIED.);
#1215=B_SPLINE_CURVE_WITH_KNOTS('',3,(#14338,#14339,#14340,#14341,#14342,
#14343),.UNSPECIFIED.,.F.,.F.,(4,1,1,4),(95.7916382276144,96.2444160663824,
97.2426107706909,97.3893722612835),.UNSPECIFIED.);
#1216=B_SPLINE_CURVE_WITH_KNOTS('',3,(#14720,#14721,#14722,#14723,#14724,
#14725,#14726,#14727,#14728,#14729,#14730,#14731,#14732,#14733,#14734,#14735,
#14736,#14737,#14738,#14739,#14740,#14741,#14742,#14743,#14744,#14745,#14746,
#14747,#14748,#14749,#14750,#14751,#14752,#14753,#14754,#14755,#14756,#14757,
#14758,#14759,#14760,#14761,#14762,#14763,#14764,#14765,#14766,#14767,#14768,
#14769,#14770,#14771,#14772,#14773,#14774,#14775,#14776,#14777,#14778,#14779,
#14780,#14781,#14782,#14783,#14784,#14785,#14786,#14787,#14788,#14789,#14790,
#14791,#14792,#14793,#14794,#14795,#14796,#14797,#14798,#14799,#14800,#14801,
#14802,#14803,#14804),.UNSPECIFIED.,.F.,.F.,(4,3,3,3,3,3,3,3,3,3,3,3,3,
3,3,3,3,3,3,3,3,3,3,3,3,3,3,3,4),(0.,0.0160334974104419,0.0395642075604872,
0.0633644118114054,0.0837263817738086,0.0874470583914756,0.1106044065324,
0.133695295128406,0.156786183724411,0.165329376229777,0.169027049684205,
0.191207839298198,0.212732869185845,0.226227078758941,0.238087469390583,
0.24288151240858,0.246186438911864,0.267772589720587,0.289583909367139,
0.305496742371809,0.315196008042082,0.319047580844878,0.340135104067482,
0.359186757307379,0.366235629765007,0.370741076209788,0.390853652067263,
0.410818111358785,0.415993328865216),.UNSPECIFIED.);
#1217=B_SPLINE_CURVE_WITH_KNOTS('',3,(#14805,#14806,#14807,#14808,#14809,
#14810,#14811,#14812,#14813,#14814,#14815,#14816,#14817,#14818,#14819,#14820,
#14821,#14822,#14823,#14824,#14825,#14826,#14827,#14828,#14829,#14830,#14831,
#14832,#14833,#14834,#14835,#14836,#14837,#14838,#14839,#14840,#14841,#14842,
#14843,#14844,#14845,#14846,#14847,#14848,#14849,#14850,#14851,#14852,#14853,
#14854,#14855,#14856,#14857,#14858,#14859,#14860,#14861,#14862,#14863,#14864,
#14865,#14866,#14867,#14868,#14869,#14870,#14871,#14872,#14873,#14874,#14875,
#14876,#14877,#14878,#14879,#14880,#14881,#14882,#14883,#14884,#14885,#14886),
 .UNSPECIFIED.,.F.,.F.,(4,3,3,3,3,3,3,3,3,3,3,3,3,3,3,3,3,3,3,3,3,3,3,3,
3,3,3,4),(-0.415993328865187,-0.402901270545643,-0.382908564830427,-0.371774763313882,
-0.367435224694355,-0.346965909888549,-0.32591580828458,-0.321433315753078,
-0.315781547589586,-0.294320173377462,-0.272479432300184,-0.257298137875953,
-0.244873415404794,-0.24111480505867,-0.218638203108128,-0.211619958938312,
-0.189699687125207,-0.167779415312101,-0.162843814523672,-0.140373337321852,
-0.117486011710451,-0.0943539309779002,-0.0856507589901794,-0.0817563326016671,
-0.0580189261100361,-0.034237541284798,-0.0109647718819074,0.),
 .UNSPECIFIED.);
#1218=B_SPLINE_CURVE_WITH_KNOTS('',3,(#14888,#14889,#14890,#14891,#14892,
#14893,#14894,#14895,#14896,#14897,#14898,#14899,#14900,#14901,#14902,#14903,
#14904,#14905,#14906,#14907,#14908,#14909,#14910,#14911,#14912,#14913,#14914,
#14915,#14916,#14917,#14918,#14919,#14920,#14921,#14922,#14923,#14924,#14925,
#14926,#14927,#14928,#14929,#14930,#14931,#14932,#14933,#14934,#14935,#14936,
#14937,#14938,#14939,#14940,#14941,#14942,#14943,#14944,#14945,#14946,#14947,
#14948,#14949,#14950,#14951,#14952,#14953,#14954,#14955,#14956,#14957,#14958,
#14959,#14960,#14961,#14962,#14963,#14964,#14965,#14966,#14967,#14968,#14969,
#14970,#14971,#14972,#14973,#14974,#14975),.UNSPECIFIED.,.F.,.F.,(4,3,3,
3,3,3,3,3,3,3,3,3,3,3,3,3,3,3,3,3,3,3,3,3,3,3,3,3,3,4),(-0.410048543780163,
-0.398139186466655,-0.374410169281135,-0.362901775202635,-0.357252904496043,
-0.353226071091677,-0.329831664544852,-0.312242260164576,-0.303769719034645,
-0.299630020912383,-0.276842045830078,-0.2545146021889,-0.232670178061085,
-0.225307920334055,-0.221146019951397,-0.21755552666877,-0.195982423137004,
-0.189116736674495,-0.166997686103039,-0.146198385794381,-0.141443407849317,
-0.120014324717733,-0.0987103641924262,-0.0775869942730841,-0.0725417907976872,
-0.0680291545044378,-0.0474611904118694,-0.02724361982139,-0.00767557047989959,
0.),.UNSPECIFIED.);
#1219=B_SPLINE_CURVE_WITH_KNOTS('',3,(#15332,#15333,#15334,#15335,#15336,
#15337,#15338,#15339,#15340,#15341,#15342,#15343,#15344,#15345,#15346,#15347,
#15348,#15349,#15350,#15351,#15352,#15353,#15354,#15355,#15356,#15357,#15358,
#15359,#15360,#15361,#15362,#15363,#15364,#15365,#15366,#15367,#15368,#15369,
#15370,#15371,#15372,#15373,#15374,#15375,#15376,#15377,#15378,#15379,#15380,
#15381,#15382,#15383,#15384,#15385,#15386,#15387,#15388,#15389,#15390,#15391,
#15392,#15393,#15394,#15395,#15396,#15397,#15398,#15399,#15400,#15401,#15402,
#15403,#15404,#15405,#15406,#15407,#15408,#15409,#15410,#15411,#15412,#15413,
#15414,#15415,#15416,#15417,#15418,#15419),.UNSPECIFIED.,.F.,.F.,(4,3,3,
3,3,3,3,3,3,3,3,3,3,3,3,3,3,3,3,3,3,3,3,3,3,3,3,3,3,4),(0.,0.0130464519754968,
0.0327301024266493,0.0529569041528836,0.0626751748968586,0.0683819350422815,
0.0728898740513483,0.0937859875900613,0.115528408032434,0.137270828474807,
0.143309507195499,0.146634619759991,0.168716970862334,0.190720450818485,
0.203657142534596,0.22030049657604,0.223957438687906,0.245775764328327,
0.268053423336898,0.290759291313493,0.295289317391233,0.299519479633725,
0.303835795791196,0.327020679917298,0.350378655359791,0.356293009821619,
0.360744190415631,0.384491412449796,0.408026460803736,0.414097116159588),
 .UNSPECIFIED.);
#1220=B_SPLINE_CURVE_WITH_KNOTS('',3,(#15544,#15545,#15546,#15547,#15548,
#15549,#15550,#15551,#15552,#15553,#15554,#15555,#15556,#15557),
 .UNSPECIFIED.,.F.,.F.,(4,2,2,2,2,2,4),(-0.844212290556731,-0.730966332817565,
-0.619975754240938,-0.457326579004558,-0.29977928179387,-0.147336283383114,
0.),.UNSPECIFIED.);
#1221=B_SPLINE_CURVE_WITH_KNOTS('',3,(#15561,#15562,#15563,#15564,#15565,
#15566,#15567,#15568,#15569,#15570,#15571,#15572,#15573,#15574),
 .UNSPECIFIED.,.F.,.F.,(4,2,2,2,2,2,4),(-0.844212290556731,-0.730966332817565,
-0.619975754240938,-0.457326579004558,-0.29977928179387,-0.147336283383114,
0.),.UNSPECIFIED.);
#1222=B_SPLINE_CURVE_WITH_KNOTS('',3,(#15611,#15612,#15613,#15614,#15615,
#15616,#15617,#15618,#15619,#15620,#15621,#15622,#15623,#15624),
 .UNSPECIFIED.,.F.,.F.,(4,2,2,2,2,2,4),(-0.847325527525843,-0.749719327139836,
-0.649860858750851,-0.495073659399383,-0.335166304629316,-0.170141007879843,
0.),.UNSPECIFIED.);
#1223=B_SPLINE_CURVE_WITH_KNOTS('',3,(#15626,#15627,#15628,#15629,#15630,
#15631,#15632,#15633,#15634,#15635,#15636,#15637,#15638,#15639),
 .UNSPECIFIED.,.F.,.F.,(4,2,2,2,2,2,4),(-0.847325527525843,-0.749719327139836,
-0.649860858750851,-0.495073659399383,-0.335166304629316,-0.170141007879843,
0.),.UNSPECIFIED.);
#1224=B_SPLINE_CURVE_WITH_KNOTS('',3,(#15688,#15689,#15690,#15691,#15692,
#15693,#15694,#15695,#15696,#15697,#15698,#15699,#15700,#15701,#15702,#15703,
#15704,#15705,#15706,#15707,#15708,#15709,#15710,#15711,#15712,#15713,#15714,
#15715,#15716,#15717,#15718,#15719,#15720,#15721,#15722,#15723,#15724,#15725,
#15726,#15727,#15728,#15729,#15730,#15731,#15732,#15733,#15734,#15735,#15736,
#15737,#15738,#15739,#15740,#15741,#15742,#15743,#15744,#15745,#15746,#15747,
#15748,#15749,#15750,#15751,#15752,#15753,#15754,#15755,#15756,#15757,#15758,
#15759,#15760,#15761,#15762,#15763,#15764,#15765,#15766,#15767,#15768,#15769,
#15770,#15771,#15772,#15773,#15774,#15775,#15776,#15777,#15778,#15779,#15780,
#15781,#15782,#15783,#15784,#15785,#15786,#15787,#15788,#15789,#15790,#15791,
#15792,#15793,#15794,#15795,#15796,#15797,#15798,#15799,#15800,#15801,#15802,
#15803,#15804,#15805,#15806,#15807,#15808,#15809,#15810,#15811,#15812,#15813,
#15814,#15815,#15816,#15817,#15818,#15819,#15820,#15821,#15822,#15823,#15824,
#15825,#15826,#15827,#15828,#15829,#15830,#15831,#15832,#15833,#15834,#15835,
#15836,#15837,#15838,#15839,#15840,#15841),.UNSPECIFIED.,.F.,.F.,(4,3,3,
3,3,3,3,3,3,3,3,3,3,3,3,3,3,3,3,3,3,3,3,3,3,3,3,3,3,3,3,3,3,3,3,3,3,3,3,
3,3,3,3,3,3,3,3,3,3,3,3,4),(10.3761051797602,10.4641373814769,10.5520588327897,
10.6410762182378,10.7288594652779,10.8166179102709,10.9043752172213,10.9943308920096,
11.0822044534747,11.1732011849246,11.2641979163745,11.3543883418031,11.4444664958327,
11.5344565843787,11.6243852832326,11.7142815564214,11.804167167181,11.8940638650899,
11.9840486455302,12.074077267802,12.1642488110667,12.247304603897,12.337349377077,
12.4272819895897,12.517126854226,12.6069114553117,12.6966643802678,12.786407578033,
12.8761629846047,12.9660091578037,13.0559004439681,13.1459382866182,13.2304112914194,
13.3202803122904,13.4100337681398,13.4996963272619,13.5892945887802,13.6788587810357,
13.7684110716423,13.8579736136466,13.947625011734,14.0373201915803,14.1271617222868,
14.2135179789419,14.3034962162208,14.3933692649306,14.4831592957879,14.5728884092593,
14.6625930287075,14.7522802792272,14.8420075718479,14.9177889943201),
 .UNSPECIFIED.);
#1225=B_SPLINE_CURVE_WITH_KNOTS('',3,(#15844,#15845,#15846,#15847,#15848,
#15849,#15850,#15851,#15852,#15853,#15854,#15855,#15856,#15857,#15858,#15859,
#15860,#15861,#15862,#15863,#15864,#15865,#15866,#15867,#15868,#15869,#15870,
#15871,#15872,#15873,#15874,#15875,#15876,#15877,#15878,#15879,#15880,#15881,
#15882,#15883,#15884,#15885,#15886,#15887,#15888,#15889,#15890,#15891,#15892,
#15893,#15894,#15895,#15896,#15897,#15898,#15899,#15900,#15901,#15902,#15903,
#15904,#15905,#15906,#15907,#15908,#15909,#15910,#15911,#15912,#15913,#15914,
#15915,#15916,#15917,#15918,#15919,#15920,#15921,#15922,#15923,#15924,#15925,
#15926,#15927,#15928,#15929,#15930,#15931,#15932,#15933,#15934,#15935,#15936,
#15937,#15938,#15939,#15940,#15941,#15942,#15943,#15944,#15945,#15946,#15947,
#15948,#15949,#15950,#15951,#15952,#15953,#15954,#15955),.UNSPECIFIED.,
 .F.,.F.,(4,3,3,3,3,3,3,3,3,3,3,3,3,3,3,3,3,3,3,3,3,3,3,3,3,3,3,3,3,3,3,
3,3,3,3,3,3,4),(11.6150691238056,11.716887748291,11.818807396451,11.9206982029579,
12.0224123053014,12.1066224675668,12.1974625342849,12.2882944241597,12.379171523673,
12.4700739203339,12.561061507472,12.598175811328,12.6891753523971,12.7800935403341,
12.8709528368157,12.9617902529354,13.0526187338464,13.1434585576012,13.2343300061399,
13.3253148905754,13.4163587789532,13.5075598865992,13.5812824988505,13.6704071444793,
13.7594059294644,13.8483044456942,13.9378150382791,14.0265967435875,14.1153607025908,
14.2041298440541,14.2941946796338,14.3830904507549,14.4737398185639,14.5643891863729,
14.6545593024114,14.7446311850219,14.8346130791444,14.9185734639323),
 .UNSPECIFIED.);
#1226=B_SPLINE_CURVE_WITH_KNOTS('',3,(#15961,#15962,#15963,#15964,#15965,
#15966,#15967,#15968,#15969,#15970,#15971,#15972,#15973,#15974,#15975,#15976,
#15977,#15978,#15979,#15980,#15981,#15982,#15983,#15984,#15985,#15986,#15987,
#15988,#15989,#15990,#15991,#15992,#15993,#15994,#15995,#15996,#15997,#15998,
#15999,#16000,#16001,#16002,#16003,#16004,#16005,#16006,#16007,#16008,#16009,
#16010,#16011,#16012,#16013,#16014,#16015,#16016,#16017,#16018,#16019,#16020,
#16021,#16022,#16023,#16024,#16025,#16026,#16027,#16028,#16029,#16030,#16031,
#16032,#16033,#16034,#16035,#16036,#16037,#16038,#16039,#16040,#16041,#16042,
#16043,#16044,#16045,#16046,#16047,#16048,#16049,#16050,#16051,#16052,#16053,
#16054,#16055,#16056,#16057,#16058,#16059,#16060,#16061,#16062,#16063,#16064,
#16065,#16066,#16067,#16068,#16069,#16070,#16071,#16072,#16073,#16074,#16075,
#16076,#16077,#16078,#16079,#16080,#16081,#16082,#16083,#16084,#16085,#16086,
#16087,#16088,#16089,#16090,#16091,#16092,#16093,#16094,#16095,#16096,#16097,
#16098,#16099,#16100,#16101,#16102,#16103,#16104,#16105,#16106,#16107,#16108,
#16109,#16110,#16111,#16112,#16113,#16114,#16115,#16116,#16117,#16118,#16119,
#16120,#16121,#16122,#16123,#16124,#16125,#16126,#16127,#16128,#16129,#16130,
#16131,#16132,#16133,#16134,#16135,#16136,#16137,#16138,#16139,#16140,#16141,
#16142,#16143,#16144,#16145,#16146,#16147),.UNSPECIFIED.,.F.,.F.,(4,3,3,
3,3,3,3,3,3,3,3,3,3,3,3,3,3,3,3,3,3,3,3,3,3,3,3,3,3,3,3,3,3,3,3,3,3,3,3,
3,3,3,3,3,3,3,3,3,3,3,3,3,3,3,3,3,3,3,3,3,3,3,4),(15.7079632680998,15.8025806359288,
15.8974688589525,15.9924919522917,16.0877730881789,16.1797313539867,16.2696858791206,
16.3595261141865,16.4492766072458,16.5389641976932,16.6286185390501,16.7182616952449,
16.8079157161731,16.8976590020199,16.9874464303251,17.0773798515868,17.1628380415092,
17.2528079127075,17.3426637193691,17.4324299876198,17.5221335971379,17.6118041005047,
17.7014635426848,17.7911339547024,17.8808936965223,17.9706976405523,18.0606475049867,
18.1459447290316,18.2359100492805,18.3257612649324,18.4155229084801,18.5052218615178,
18.5948876907088,18.6845424465949,18.7742081657681,18.8639632336747,18.9537625072052,
19.0437077565897,19.1290514165541,19.2190155261937,19.3088654988141,19.3986258687219,
19.4883235067968,19.5779879963056,19.6676413893196,19.7573057239427,19.8470593814408,
19.9368572283733,20.026801038463,20.1121581040765,20.2021239629424,20.291975712,
20.3817378830449,20.4714373523156,20.5611036906873,20.650758948064,20.7404251603941,
20.8301807051032,20.9199804472223,21.0099261460961,21.095264791599,21.1842153811775,
21.2018918374058),.UNSPECIFIED.);
#1227=B_SPLINE_CURVE_WITH_KNOTS('',3,(#16148,#16149,#16150,#16151,#16152,
#16153,#16154,#16155,#16156,#16157,#16158,#16159,#16160,#16161,#16162,#16163,
#16164,#16165,#16166,#16167,#16168,#16169,#16170,#16171,#16172,#16173,#16174,
#16175),.UNSPECIFIED.,.F.,.F.,(4,3,3,3,3,3,3,3,3,4),(14.9177889943201,15.0076144356903,
15.1021195510773,15.1966246664643,15.2902720900812,15.3837656172365,15.4770712880676,
15.5702644610989,15.6633265890774,15.707963267949),.UNSPECIFIED.);
#1228=B_SPLINE_CURVE_WITH_KNOTS('',3,(#16177,#16178,#16179,#16180,#16181,
#16182,#16183,#16184,#16185,#16186,#16187,#16188,#16189,#16190,#16191,#16192,
#16193,#16194,#16195,#16196,#16197,#16198,#16199,#16200,#16201,#16202,#16203,
#16204),.UNSPECIFIED.,.F.,.F.,(4,3,3,3,3,3,3,3,3,4),(14.9185734639323,15.0084711991854,
15.098356819238,15.188252074111,15.2782346001737,15.3682596620585,15.4584293984242,
15.5474958738954,15.6867796530317,15.707963267949),.UNSPECIFIED.);
#1229=B_SPLINE_CURVE_WITH_KNOTS('',3,(#16205,#16206,#16207,#16208,#16209,
#16210,#16211,#16212,#16213,#16214,#16215,#16216,#16217,#16218,#16219,#16220,
#16221,#16222,#16223,#16224,#16225,#16226,#16227,#16228,#16229,#16230,#16231,
#16232,#16233,#16234,#16235,#16236,#16237,#16238,#16239,#16240,#16241,#16242,
#16243,#16244,#16245,#16246,#16247,#16248,#16249,#16250,#16251,#16252,#16253,
#16254,#16255,#16256,#16257,#16258,#16259,#16260,#16261,#16262,#16263,#16264,
#16265,#16266,#16267,#16268,#16269,#16270,#16271,#16272,#16273,#16274,#16275,
#16276,#16277,#16278,#16279,#16280,#16281,#16282,#16283,#16284,#16285,#16286,
#16287,#16288,#16289,#16290,#16291,#16292,#16293,#16294,#16295,#16296,#16297,
#16298,#16299,#16300,#16301,#16302,#16303,#16304,#16305,#16306,#16307,#16308,
#16309,#16310,#16311,#16312,#16313,#16314,#16315,#16316,#16317,#16318,#16319,
#16320,#16321,#16322,#16323,#16324,#16325,#16326,#16327,#16328,#16329,#16330,
#16331,#16332,#16333,#16334,#16335,#16336,#16337,#16338,#16339,#16340,#16341,
#16342,#16343,#16344,#16345,#16346,#16347,#16348),.UNSPECIFIED.,.F.,.F.,
(4,2,2,2,2,2,2,2,2,2,2,2,2,2,2,2,2,2,2,2,2,2,2,2,2,2,2,2,2,2,2,2,2,2,2,
2,2,2,2,2,2,2,2,2,2,2,2,2,2,2,2,2,2,2,2,2,2,2,2,2,2,2,2,2,2,2,2,2,2,2,2,
4),(-4.68834833989019,-4.65508458841591,-4.59936853516785,-4.5790813115814,
-4.56541263893702,-4.55313285952382,-4.53301523131224,-4.45452755219641,
-4.41709446190139,-4.39439056254963,-4.38478358651806,-4.37733830672561,
-4.36755283705401,-4.34526465960844,-4.26412972485333,-4.23599109014725,
-4.21340244336273,-4.19937405149395,-4.18607249207315,-4.16685171300768,
-4.08269551421159,-4.03611632283646,-4.02238977108734,-4.01437018657326,
-4.00632509367964,-3.99262969623786,-3.91813590387533,-3.86390045301744,
-3.84377785905482,-3.83011327226075,-3.817768394177,-3.79736383803744,-3.74525121754264,
-3.69946993342188,-3.67540166413208,-3.65835341595994,-3.6496444466923,
-3.64206686067612,-3.63050541430058,-3.59036829320484,-3.52605167574737,
-3.50022522337047,-3.47895023408489,-3.46511273157843,-3.45139484396221,
-3.43079594325119,-3.37345492623386,-3.32263607034887,-3.3039700925282,
-3.28972990718864,-3.28158527710179,-3.27363598766241,-3.26037006749997,
-3.19786218381033,-3.13570202782019,-3.11324768666422,-3.09919903590241,
-3.08580451090809,-3.06630060367248,-2.98415154633769,-2.93656061137152,
-2.92269674301749,-2.9146263038001,-2.90659908334924,-2.89296577665551,
-2.81812796262566,-2.77158728473206,-2.74773243946704,-2.73341867447911,
-2.71999272674547,-2.70120049750362,-2.63911108106228),.UNSPECIFIED.);
#1230=B_SPLINE_CURVE_WITH_KNOTS('',3,(#16354,#16355,#16356,#16357,#16358,
#16359,#16360,#16361,#16362,#16363,#16364,#16365,#16366,#16367,#16368,#16369,
#16370,#16371,#16372,#16373,#16374,#16375,#16376,#16377,#16378,#16379,#16380,
#16381,#16382,#16383,#16384,#16385,#16386,#16387,#16388,#16389,#16390,#16391,
#16392,#16393,#16394,#16395,#16396,#16397,#16398,#16399,#16400,#16401,#16402,
#16403,#16404,#16405,#16406,#16407,#16408,#16409,#16410,#16411,#16412,#16413,
#16414,#16415,#16416,#16417,#16418,#16419,#16420,#16421,#16422,#16423,#16424,
#16425,#16426,#16427,#16428,#16429,#16430,#16431,#16432,#16433,#16434,#16435,
#16436,#16437,#16438,#16439,#16440,#16441,#16442,#16443,#16444,#16445,#16446,
#16447,#16448,#16449,#16450,#16451,#16452,#16453,#16454,#16455,#16456,#16457,
#16458,#16459,#16460,#16461,#16462,#16463,#16464,#16465,#16466,#16467,#16468,
#16469,#16470,#16471,#16472,#16473,#16474,#16475,#16476,#16477,#16478,#16479,
#16480,#16481,#16482,#16483,#16484,#16485,#16486,#16487,#16488,#16489,#16490,
#16491,#16492,#16493,#16494,#16495,#16496,#16497,#16498,#16499,#16500,#16501,
#16502,#16503,#16504,#16505),.UNSPECIFIED.,.F.,.F.,(4,2,2,2,2,2,2,2,2,2,
2,2,2,2,2,2,2,2,2,2,2,2,2,2,2,2,2,2,2,2,2,2,2,2,2,2,2,2,2,2,2,2,2,2,2,2,
2,2,2,2,2,2,2,2,2,2,2,2,2,2,2,2,2,2,2,2,2,2,2,2,2,2,2,2,2,4),(-2.04961240608362,
-2.04846731799055,-2.03436004178467,-2.01161307201698,-1.95901316641739,
-1.88542547187917,-1.87319853180591,-1.86620666267941,-1.85804905011015,
-1.84376392206717,-1.8250195380913,-1.77373456495123,-1.71718578570372,
-1.69662030237994,-1.68290586402199,-1.66905647746236,-1.64773020420228,
-1.6218186176251,-1.55705364820425,-1.5172871902438,-1.50578779123524,-1.4982284826178,
-1.48953471339632,-1.47247022460861,-1.44835840631695,-1.40249579092161,
-1.3502259145096,-1.32981793099076,-1.31749643676501,-1.30388097758378,
-1.28388892440881,-1.23041687198386,-1.15449633129897,-1.14103176949053,
-1.13303956077813,-1.12492937753314,-1.11088048165017,-1.06161796178586,
-0.982327429975348,-0.962466786186025,-0.949008683269062,-0.935038023101868,
-0.913039766196341,-0.885971894866213,-0.813642258455964,-0.782550486682968,
-0.771683320463845,-0.764134892944955,-0.755084673027459,-0.736010379366222,
-0.707570669679222,-0.614163672308585,-0.594951686439576,-0.581598840138717,
-0.567460480065028,-0.544540495207097,-0.488926516689361,-0.419679077959112,
-0.406953607062545,-0.39987805797259,-0.391854521371385,-0.378232422063269,
-0.332772474241522,-0.246975016100116,-0.227977242725061,-0.214657643796333,
-0.200455991100291,-0.177189922589633,-0.126906508617021,-0.119577861397492,
-0.0540343017638599,-0.0407615282157486,-0.0328081263525258,-0.0259069908760486,
-0.0150954331368796,-0.000789799928729903),.UNSPECIFIED.);
#1231=B_SPLINE_CURVE_WITH_KNOTS('',3,(#16506,#16507,#16508,#16509,#16510,
#16511,#16512,#16513,#16514,#16515,#16516,#16517,#16518,#16519,#16520,#16521,
#16522,#16523,#16524,#16525,#16526,#16527,#16528,#16529,#16530,#16531,#16532,
#16533),.UNSPECIFIED.,.F.,.F.,(4,3,3,3,3,3,3,3,3,4),(21.2018918374058,21.2907068140922,
21.3794336288738,21.4681122919233,21.556765901624,21.6454175303288,21.7341402280128,
21.8228977713556,21.9117857326907,21.9911485748867),.UNSPECIFIED.);
#1232=B_SPLINE_CURVE_WITH_KNOTS('',3,(#16534,#16535,#16536,#16537,#16538,
#16539,#16540,#16541,#16542,#16543,#16544,#16545,#16546,#16547,#16548,#16549,
#16550,#16551,#16552,#16553,#16554,#16555,#16556,#16557,#16558,#16559,#16560,
#16561,#16562,#16563,#16564,#16565,#16566,#16567,#16568,#16569,#16570,#16571,
#16572,#16573,#16574,#16575,#16576,#16577,#16578,#16579,#16580,#16581,#16582,
#16583,#16584,#16585,#16586,#16587,#16588,#16589,#16590,#16591,#16592,#16593,
#16594,#16595,#16596,#16597,#16598,#16599,#16600,#16601,#16602,#16603,#16604,
#16605,#16606,#16607,#16608,#16609,#16610,#16611,#16612,#16613,#16614,#16615,
#16616,#16617,#16618,#16619,#16620,#16621,#16622,#16623,#16624,#16625,#16626,
#16627,#16628,#16629,#16630,#16631,#16632,#16633,#16634,#16635,#16636,#16637,
#16638,#16639,#16640,#16641,#16642,#16643,#16644,#16645,#16646,#16647,#16648,
#16649,#16650,#16651,#16652,#16653,#16654,#16655,#16656,#16657,#16658,#16659,
#16660,#16661,#16662,#16663,#16664,#16665,#16666,#16667,#16668,#16669,#16670,
#16671,#16672,#16673,#16674,#16675,#16676,#16677,#16678,#16679,#16680,#16681,
#16682,#16683,#16684,#16685,#16686,#16687,#16688,#16689,#16690,#16691,#16692,
#16693,#16694,#16695,#16696,#16697,#16698,#16699,#16700,#16701,#16702,#16703,
#16704,#16705,#16706,#16707),.UNSPECIFIED.,.F.,.F.,(4,2,2,2,2,2,2,2,2,2,
2,2,2,2,2,2,2,2,2,2,2,2,2,2,2,2,2,2,2,2,2,2,2,2,2,2,2,2,2,2,2,2,2,2,2,2,
2,2,2,2,2,2,2,2,2,2,2,2,2,2,2,2,2,2,2,2,2,2,2,2,2,2,2,2,2,2,2,2,2,2,2,2,
2,2,2,2,4),(-2.63911108106228,-2.61389722979619,-2.58107538358811,-2.5601522761232,
-2.550795983286,-2.54328991325651,-2.53288104898045,-2.50600697108263,-2.4295932887207,
-2.38954025089258,-2.37273638949239,-2.35967215395335,-2.34446025202537,
-2.31550887548481,-2.27478735054413,-2.20378467546804,-2.18955829491125,
-2.18141270854979,-2.17345219573091,-2.16014719142536,-2.14315008517139,
-2.10088252274014,-2.03204595619649,-2.01134104316741,-1.99760171142334,
-1.98377849291404,-1.9626008425893,-1.93694244287669,-1.87367392801601,
-1.83199842659466,-1.82042487480467,-1.81285385872645,-1.80419083149189,
-1.78729624834157,-1.76353300680594,-1.66860729576893,-1.64625056094355,
-1.6322141983133,-1.61864286052398,-1.59891660989387,-1.53138463918856,
-1.46857629414052,-1.45531358220379,-1.44736134632962,-1.43920489637716,
-1.42492578659526,-1.40619239993965,-1.3549702034927,-1.29834119110781,
-1.27777341702507,-1.26405860720962,-1.25020973837015,-1.22888621542746,
-1.20297938762556,-1.13824420357628,-1.0984372513944,-1.08693609302705,
-1.07937656536868,-1.07068367372916,-1.05362397636827,-1.02952203417856,
-0.98364443777249,-0.931370926167948,-0.910962639701207,-0.898641060894736,
-0.885025586405433,-0.865033684567714,-0.81156307559681,-0.735639094077008,
-0.722174965910665,-0.714182807345869,-0.706072383932551,-0.692022659349403,
-0.642753345690428,-0.563473062628527,-0.543610957050241,-0.530152467778737,
-0.516181876455237,-0.4941847686508,-0.467119020859666,-0.394805623179322,
-0.363695858756982,-0.352826988555971,-0.345278305435169,-0.336228972575739,
-0.31715997569338,-0.295509696228243),.UNSPECIFIED.);
#1233=B_SPLINE_CURVE_WITH_KNOTS('',3,(#16712,#16713,#16714,#16715,#16716,
#16717,#16718,#16719,#16720,#16721,#16722,#16723,#16724,#16725,#16726,#16727,
#16728,#16729,#16730,#16731,#16732,#16733,#16734,#16735,#16736,#16737,#16738,
#16739,#16740,#16741,#16742,#16743,#16744,#16745,#16746,#16747,#16748,#16749,
#16750,#16751,#16752,#16753,#16754,#16755,#16756,#16757,#16758,#16759,#16760,
#16761,#16762,#16763,#16764,#16765,#16766,#16767,#16768,#16769,#16770,#16771,
#16772,#16773,#16774,#16775,#16776,#16777,#16778,#16779,#16780,#16781,#16782,
#16783,#16784,#16785,#16786,#16787,#16788,#16789,#16790,#16791,#16792,#16793,
#16794,#16795,#16796,#16797,#16798,#16799,#16800,#16801,#16802,#16803,#16804,
#16805,#16806,#16807,#16808,#16809,#16810,#16811,#16812,#16813,#16814,#16815,
#16816,#16817,#16818,#16819,#16820,#16821,#16822,#16823,#16824,#16825,#16826,
#16827,#16828,#16829,#16830,#16831,#16832,#16833,#16834,#16835,#16836,#16837,
#16838,#16839,#16840,#16841,#16842,#16843,#16844,#16845,#16846,#16847,#16848,
#16849,#16850,#16851,#16852,#16853,#16854,#16855,#16856,#16857,#16858,#16859,
#16860,#16861,#16862,#16863,#16864,#16865,#16866,#16867,#16868,#16869,#16870,
#16871,#16872,#16873,#16874,#16875,#16876,#16877,#16878,#16879,#16880,#16881),
 .UNSPECIFIED.,.F.,.F.,(4,2,2,2,2,2,2,2,2,2,2,2,2,2,2,2,2,2,2,2,2,2,2,2,
2,2,2,2,2,2,2,2,2,2,2,2,2,2,2,2,2,2,2,2,2,2,2,2,2,2,2,2,2,2,2,2,2,2,2,2,
2,2,2,2,2,2,2,2,2,2,2,2,2,2,2,2,2,2,2,2,2,2,2,2,4),(-4.39331191224356,-4.37560145592145,
-4.3114098378457,-4.28559723109706,-4.26432706433371,-4.25048666776118,
-4.23676120924672,-4.2161396052254,-4.15758212839039,-4.10780046029863,
-4.08932156506745,-4.07518332955413,-4.06705468353004,-4.05907733379765,
-4.04569037808528,-3.96933062871353,-3.91612022710783,-3.89616390726823,
-3.88255322030396,-3.87022374256306,-3.84977313359501,-3.77616507531547,
-3.71850135239065,-3.70650134333133,-3.69878481714542,-3.69025645248449,
-3.67407947539339,-3.64217220063643,-3.57796963814975,-3.55215538960743,
-3.53088434176985,-3.51704392408621,-3.50331884229407,-3.48269860268792,
-3.42419311520387,-3.37437279924298,-3.35588700498925,-3.3417450061456,
-3.33361567696377,-3.32563914287365,-3.31225590056248,-3.23587587640272,
-3.18267746757575,-3.16272300834602,-3.14911278114548,-3.13678321930216,
-3.1163312519161,-3.06325580215698,-3.00912957786561,-2.98134994717596,
-2.97106215474424,-2.96356598998976,-2.95412369418129,-2.93263443394907,
-2.84990538773865,-2.8215710499691,-2.79885016675484,-2.78474706393444,
-2.77137168957434,-2.75202549340976,-2.6686528381238,-2.63410367221121,
-2.61888788716139,-2.60662398920565,-2.59886141854827,-2.5904255250284,
-2.574729418821,-2.49848379943591,-2.46222890543053,-2.4353573334932,-2.42050346161586,
-2.40725506197321,-2.39007210853799,-2.34835036770994,-2.34385649726276,
-2.30125828656882,-2.25500136049857,-2.24127765538967,-2.23323329900269,
-2.22517822282473,-2.21140203063287,-2.16460737724514,-2.0811651465222,
-2.06183878417439,-2.04961240608362),.UNSPECIFIED.);
#1234=B_SPLINE_CURVE_WITH_KNOTS('',3,(#16883,#16884,#16885,#16886,#16887,
#16888,#16889,#16890,#16891,#16892,#16893,#16894,#16895,#16896,#16897,#16898,
#16899,#16900,#16901,#16902),.UNSPECIFIED.,.F.,.F.,(4,2,2,2,2,2,2,2,2,4),
(-0.295509696228243,-0.288732319901063,-0.195289147016525,-0.176083510006063,
-0.162731641333534,-0.148591438424712,-0.125661485943037,-0.0784178946907411,
-0.0433454634721789,-0.000849774496175227),.UNSPECIFIED.);
#1235=B_SPLINE_CURVE_WITH_KNOTS('',3,(#16903,#16904,#16905,#16906,#16907,
#16908,#16909,#16910,#16911,#16912,#16913,#16914,#16915,#16916,#16917,#16918,
#16919,#16920,#16921,#16922,#16923,#16924,#16925,#16926,#16927,#16928,#16929,
#16930,#16931,#16932,#16933,#16934,#16935,#16936,#16937,#16938,#16939,#16940,
#16941,#16942,#16943,#16944,#16945,#16946,#16947,#16948,#16949,#16950,#16951,
#16952,#16953,#16954,#16955,#16956,#16957,#16958,#16959,#16960,#16961,#16962,
#16963,#16964,#16965,#16966,#16967,#16968,#16969,#16970,#16971,#16972,#16973,
#16974,#16975,#16976,#16977,#16978,#16979,#16980,#16981,#16982,#16983,#16984,
#16985,#16986,#16987,#16988,#16989,#16990,#16991,#16992,#16993,#16994,#16995,
#16996,#16997,#16998,#16999,#17000,#17001,#17002,#17003,#17004,#17005,#17006,
#17007,#17008,#17009,#17010,#17011,#17012,#17013,#17014,#17015,#17016,#17017,
#17018,#17019,#17020,#17021,#17022,#17023,#17024,#17025,#17026,#17027,#17028,
#17029,#17030,#17031,#17032,#17033,#17034,#17035,#17036,#17037,#17038,#17039,
#17040,#17041,#17042,#17043,#17044,#17045,#17046,#17047,#17048),
 .UNSPECIFIED.,.F.,.F.,(4,2,2,2,2,2,2,2,2,2,2,2,2,2,2,2,2,2,2,2,2,2,2,2,
2,2,2,2,2,2,2,2,2,2,2,2,2,2,2,2,2,2,2,2,2,2,2,2,2,2,2,2,2,2,2,2,2,2,2,2,
2,2,2,2,2,2,2,2,2,2,2,2,4),(-4.68759801305522,-4.6786154966478,-4.67025567535162,
-4.6628645751344,-4.65223210683701,-4.62317292131303,-4.59213647822212,
-4.52143234373722,-4.49938333712422,-4.48540599860914,-4.47195826986589,
-4.45214546014359,-4.37245518818805,-4.32342159994108,-4.30939887528759,
-4.30129530818617,-4.29330073673223,-4.27981849315781,-4.20409229043172,
-4.15057732839138,-4.13058263478209,-4.11696897906048,-4.10465114727064,
-4.0842547132693,-4.03221306536484,-3.97725754120375,-3.95789045640485,
-3.94326715242319,-3.93504326786529,-3.92714848444638,-3.91417148670484,
-3.84726916472332,-3.78980183252394,-3.76692840033962,-3.75280000279642,
-3.73944452763723,-3.72020714318806,-3.6360969864323,-3.58966282756493,
-3.5759287196203,-3.56788324248193,-3.56082448852716,-3.54819342919581,
-3.47820160032019,-3.42252834510268,-3.39998001298162,-3.38591079074289,
-3.37252052124575,-3.35306586152839,-3.27055413659815,-3.22319745262476,
-3.20935867548291,-3.20129183736159,-3.19424689712922,-3.18169770743099,
-3.11098978407951,-3.06832188780665,-3.03852247171375,-3.02317149459409,
-3.00999824711346,-2.99332968738289,-2.95718388232658,-2.89082012494614,
-2.85159959278265,-2.84030044630581,-2.83269667724201,-2.82387792395333,
-2.80612186603167,-2.73236496483843,-2.67943159839657,-2.66144687690544,
-2.6481406310148,-2.63907567363619),.UNSPECIFIED.);
#1236=B_SPLINE_CURVE_WITH_KNOTS('',3,(#17054,#17055,#17056,#17057,#17058,
#17059,#17060,#17061,#17062,#17063,#17064,#17065,#17066,#17067,#17068,#17069,
#17070,#17071,#17072,#17073,#17074,#17075,#17076,#17077,#17078,#17079,#17080,
#17081,#17082,#17083,#17084,#17085,#17086,#17087,#17088,#17089,#17090,#17091,
#17092,#17093,#17094,#17095,#17096,#17097,#17098,#17099,#17100,#17101,#17102,
#17103,#17104,#17105,#17106,#17107,#17108,#17109,#17110,#17111,#17112,#17113,
#17114,#17115,#17116,#17117,#17118,#17119,#17120,#17121,#17122,#17123,#17124,
#17125,#17126,#17127,#17128,#17129,#17130,#17131,#17132,#17133,#17134,#17135,
#17136,#17137,#17138,#17139,#17140,#17141,#17142,#17143,#17144,#17145,#17146,
#17147,#17148,#17149,#17150,#17151,#17152,#17153,#17154,#17155,#17156,#17157,
#17158,#17159,#17160,#17161,#17162,#17163,#17164,#17165,#17166,#17167,#17168,
#17169,#17170,#17171,#17172,#17173,#17174,#17175,#17176,#17177,#17178,#17179,
#17180,#17181,#17182,#17183,#17184,#17185,#17186,#17187,#17188,#17189,#17190,
#17191,#17192,#17193,#17194,#17195,#17196,#17197,#17198,#17199,#17200,#17201),
 .UNSPECIFIED.,.F.,.F.,(4,2,2,2,2,2,2,2,2,2,2,2,2,2,2,2,2,2,2,2,2,2,2,2,
2,2,2,2,2,2,2,2,2,2,2,2,2,2,2,2,2,2,2,2,2,2,2,2,2,2,2,2,2,2,2,2,2,2,2,2,
2,2,2,2,2,2,2,2,2,2,2,2,2,4),(-2.04935972616353,-2.00287868864084,-1.96348539660213,
-1.95200435192754,-1.94437392958132,-1.93564018773703,-1.91835400231652,
-1.89378364346478,-1.82847651371751,-1.78860668362923,-1.77170794880324,
-1.75849218522515,-1.74347937011549,-1.71568714435376,-1.67749745058458,
-1.60037752081791,-1.58711454399874,-1.57916308051959,-1.57100770911776,
-1.5567326033437,-1.53800606871541,-1.48681916417169,-1.43015414516619,
-1.40958628073977,-1.39587173439376,-1.38202329951776,-1.36070058607619,
-1.33479451720022,-1.27005605998517,-1.23011621418989,-1.21868834586002,
-1.21106512230926,-1.20230541250574,-1.18487847669069,-1.16001557566708,
-1.0929767775654,-1.05499434189848,-1.03822663041946,-1.02502320336602,
-1.00992791218209,-0.981656924503879,-0.942434965128106,-0.867914165428893,
-0.85422610342954,-0.846189507761945,-0.838128212684673,-0.824318846986697,
-0.777223782108126,-0.69431711325095,-0.674921111776785,-0.661539525701319,
-0.647453112958258,-0.624815189644104,-0.596623704581938,-0.515252020022513,
-0.493211842317082,-0.483437121690746,-0.475956048139001,-0.466225246491797,
-0.442774749118955,-0.40318202197825,-0.329983945530972,-0.309512549739534,
-0.297181605479188,-0.283577339444177,-0.263648092338427,-0.210617963199273,
-0.133874640825955,-0.120547771633543,-0.112583317500223,-0.104442666036868,
-0.090240784549733,-0.071647175289315,-0.000795291253163828),
 .UNSPECIFIED.);
#1237=B_SPLINE_CURVE_WITH_KNOTS('',3,(#17202,#17203,#17204,#17205,#17206,
#17207,#17208,#17209,#17210,#17211,#17212,#17213,#17214,#17215,#17216,#17217,
#17218,#17219,#17220,#17221,#17222,#17223,#17224,#17225,#17226,#17227),
 .UNSPECIFIED.,.F.,.F.,(4,2,2,2,2,2,2,2,2,2,2,2,4),(-4.68819911033501,-4.64525715217843,
-4.63117657311148,-4.6173221871197,-4.60361287686467,-4.58307549428896,
-4.48482308210793,-4.46082893190692,-4.44382216683465,-4.43513850354181,
-4.42757461095918,-4.41604906773608,-4.39331191224356),.UNSPECIFIED.);
#1238=B_SPLINE_CURVE_WITH_KNOTS('',3,(#17228,#17229,#17230,#17231,#17232,
#17233,#17234,#17235,#17236,#17237,#17238,#17239,#17240,#17241,#17242,#17243,
#17244,#17245,#17246,#17247,#17248,#17249,#17250,#17251,#17252,#17253,#17254,
#17255,#17256,#17257,#17258,#17259,#17260,#17261,#17262,#17263,#17264,#17265,
#17266,#17267,#17268,#17269,#17270,#17271,#17272,#17273,#17274,#17275,#17276,
#17277,#17278,#17279,#17280,#17281,#17282,#17283,#17284,#17285,#17286,#17287,
#17288,#17289,#17290,#17291,#17292,#17293,#17294,#17295,#17296,#17297,#17298,
#17299,#17300,#17301,#17302,#17303,#17304,#17305,#17306,#17307,#17308,#17309,
#17310,#17311,#17312,#17313,#17314,#17315,#17316,#17317,#17318,#17319,#17320,
#17321,#17322,#17323,#17324,#17325,#17326,#17327,#17328,#17329,#17330,#17331,
#17332,#17333,#17334,#17335,#17336,#17337,#17338,#17339,#17340,#17341,#17342,
#17343,#17344,#17345,#17346,#17347,#17348,#17349,#17350,#17351,#17352,#17353,
#17354,#17355,#17356,#17357,#17358,#17359,#17360,#17361,#17362,#17363,#17364,
#17365,#17366,#17367,#17368,#17369,#17370,#17371,#17372,#17373,#17374,#17375,
#17376,#17377,#17378,#17379,#17380,#17381,#17382,#17383,#17384,#17385,#17386,
#17387,#17388,#17389,#17390,#17391),.UNSPECIFIED.,.F.,.F.,(4,2,2,2,2,2,
2,2,2,2,2,2,2,2,2,2,2,2,2,2,2,2,2,2,2,2,2,2,2,2,2,2,2,2,2,2,2,2,2,2,2,2,
2,2,2,2,2,2,2,2,2,2,2,2,2,2,2,2,2,2,2,2,2,2,2,2,2,2,2,2,2,2,2,2,2,2,2,2,
2,2,2,4),(-2.63907567363619,-2.63353064505958,-2.60801751905643,-2.51818800140292,
-2.49479434972446,-2.47808392415393,-2.46945635872354,-2.46187412559938,
-2.4502223575671,-2.40612004016064,-2.34478194314754,-2.30928323673228,
-2.2926220067423,-2.27944848095648,-2.26409046468512,-2.23425393364265,
-2.19149993939338,-2.12089221799156,-2.10832363955171,-2.10127501114432,
-2.09321211442392,-2.07939549960996,-2.03223776300458,-1.94943690180683,
-1.93002619597174,-1.91664203229402,-1.90255915283176,-1.87994177010337,
-1.85178694147416,-1.7707496135778,-1.74841606446426,-1.73859433539439,
-1.73111211809046,-1.72142614200125,-1.69829122941282,-1.65960041540032,
-1.58477467030498,-1.5644394207457,-1.55212975652146,-1.53850310778816,
-1.51844223550693,-1.46447164355286,-1.38948677230892,-1.37587171732104,
-1.36784953210292,-1.35977237914557,-1.34588590918342,-1.29810522081131,
-1.21636511959362,-1.19681330354961,-1.18340621499847,-1.16936013767159,
-1.14694547490303,-1.08421091076134,-1.02219894994912,-1.00890328300781,
-1.00094508148897,-0.992797233755798,-0.978559498632532,-0.959900844567123,
-0.909097408675758,-0.851941088797705,-0.831359631322577,-0.81764288970605,
-0.803797493844524,-0.782490762786256,-0.756611941812649,-0.692038181975799,
-0.65215359208302,-0.640590333439407,-0.633021623663755,-0.624356235392163,
-0.607443723800613,-0.583642199543344,-0.537336869832293,-0.484974895067171,
-0.464563490487046,-0.452241981576471,-0.438628053287245,-0.418641583518384,
-0.365204452142173,-0.295612647763091),.UNSPECIFIED.);
#1239=B_SPLINE_CURVE_WITH_KNOTS('',3,(#17396,#17397,#17398,#17399,#17400,
#17401,#17402,#17403,#17404,#17405,#17406,#17407,#17408,#17409,#17410,#17411,
#17412,#17413,#17414,#17415,#17416,#17417,#17418,#17419,#17420,#17421,#17422,
#17423,#17424,#17425,#17426,#17427,#17428,#17429,#17430,#17431,#17432,#17433,
#17434,#17435,#17436,#17437,#17438,#17439,#17440,#17441,#17442,#17443,#17444,
#17445,#17446,#17447,#17448,#17449,#17450,#17451,#17452,#17453,#17454,#17455,
#17456,#17457,#17458,#17459,#17460,#17461,#17462,#17463,#17464,#17465,#17466,
#17467,#17468,#17469,#17470,#17471,#17472,#17473,#17474,#17475,#17476,#17477,
#17478,#17479,#17480,#17481,#17482,#17483,#17484,#17485,#17486,#17487,#17488,
#17489,#17490,#17491,#17492,#17493,#17494,#17495,#17496,#17497,#17498,#17499,
#17500,#17501,#17502,#17503,#17504,#17505,#17506,#17507,#17508,#17509,#17510,
#17511,#17512,#17513,#17514,#17515,#17516,#17517,#17518,#17519,#17520,#17521,
#17522,#17523,#17524,#17525,#17526,#17527,#17528,#17529,#17530,#17531,#17532,
#17533,#17534,#17535,#17536,#17537,#17538,#17539,#17540,#17541,#17542,#17543,
#17544,#17545,#17546,#17547,#17548,#17549,#17550,#17551,#17552,#17553,#17554,
#17555,#17556,#17557,#17558,#17559,#17560,#17561,#17562,#17563,#17564,#17565),
 .UNSPECIFIED.,.F.,.F.,(4,2,2,2,2,2,2,2,2,2,2,2,2,2,2,2,2,2,2,2,2,2,2,2,
2,2,2,2,2,2,2,2,2,2,2,2,2,2,2,2,2,2,2,2,2,2,2,2,2,2,2,2,2,2,2,2,2,2,2,2,
2,2,2,2,2,2,2,2,2,2,2,2,2,2,2,2,2,2,2,2,2,2,2,2,4),(-4.39249448366002,-4.39228442382296,
-4.36624522775283,-4.34485517680281,-4.33099492328683,-4.31729089254084,
-4.29679124486917,-4.24399423786801,-4.172528765972,-4.15602898563903,-4.14745955520206,
-4.13991509140376,-4.12831425695246,-4.08789120042157,-4.02379879994784,
-3.99803204674711,-3.97681200166545,-3.9630349475578,-3.94940204568254,
-3.92899435544657,-3.85525075729416,-3.81579601526264,-3.79240788871937,
-3.78271487454789,-3.77524925625372,-3.76548718305355,-3.74352427155699,
-3.66209112923551,-3.63388215347115,-3.61121976053594,-3.59710457897656,
-3.58368272597902,-3.56419577308114,-3.47257812657962,-3.44365114130089,
-3.42435936505704,-3.41525470764449,-3.40769761272765,-3.39684962061223,
-3.36599748914682,-3.29354789752857,-3.26647814779013,-3.24448123979525,
-3.23051506763327,-3.21706384211106,-3.19722018365833,-3.11760336747554,
-3.06841041023518,-3.05437157203105,-3.04626818824091,-3.0382849418778,
-3.02484490256617,-2.94885975518951,-2.89546622904403,-2.87549195522435,
-2.86188643880914,-2.84957298542905,-2.82917792216145,-2.77709802182455,
-2.70079830107649,-2.68727129968986,-2.67926965420796,-2.67117489870268,
-2.65720358177509,-2.60457039569869,-2.53390708957793,-2.51142016148291,
-2.49735857056104,-2.48395523679781,-2.46444270405563,-2.37267539332504,
-2.34364890820992,-2.32431707470038,-2.31522133147941,-2.30843999794085,
-2.29821281914258,-2.27093899867751,-2.21874914374114,-2.16336653594517,
-2.14283376699984,-2.12912626819679,-2.11527268489251,-2.09391646697886,
-2.06795334450763,-2.04935972616353),.UNSPECIFIED.);
#1240=B_SPLINE_CURVE_WITH_KNOTS('',3,(#17567,#17568,#17569,#17570,#17571,
#17572,#17573,#17574,#17575,#17576,#17577,#17578,#17579,#17580,#17581,#17582,
#17583,#17584,#17585,#17586,#17587,#17588,#17589,#17590,#17591,#17592),
 .UNSPECIFIED.,.F.,.F.,(4,2,2,2,2,2,2,2,2,2,2,2,4),(-0.295612647763091,
-0.289227568051325,-0.275773653121545,-0.267783893754413,-0.259672125375975,
-0.245613574134191,-0.196256444162708,-0.116878554200494,-0.0971127347560032,
-0.0836709007961119,-0.069678723514285,-0.0553703118653591,-0.000790905559261049),
 .UNSPECIFIED.);
#1241=B_SPLINE_CURVE_WITH_KNOTS('',3,(#17593,#17594,#17595,#17596,#17597,
#17598,#17599,#17600,#17601,#17602,#17603,#17604,#17605,#17606,#17607,#17608,
#17609,#17610,#17611,#17612,#17613,#17614,#17615,#17616,#17617,#17618,#17619,
#17620,#17621,#17622,#17623,#17624,#17625,#17626,#17627,#17628,#17629,#17630,
#17631,#17632,#17633,#17634,#17635,#17636,#17637,#17638,#17639,#17640,#17641,
#17642,#17643,#17644,#17645,#17646,#17647,#17648,#17649,#17650,#17651,#17652,
#17653,#17654,#17655,#17656,#17657,#17658,#17659,#17660,#17661,#17662,#17663,
#17664,#17665,#17666,#17667,#17668,#17669,#17670,#17671,#17672,#17673,#17674,
#17675,#17676,#17677,#17678,#17679,#17680,#17681,#17682,#17683,#17684,#17685,
#17686,#17687,#17688,#17689,#17690,#17691,#17692,#17693,#17694,#17695,#17696,
#17697,#17698,#17699,#17700,#17701,#17702,#17703,#17704,#17705,#17706,#17707,
#17708,#17709,#17710,#17711,#17712,#17713,#17714,#17715,#17716,#17717,#17718,
#17719,#17720,#17721,#17722,#17723,#17724,#17725,#17726,#17727,#17728,#17729,
#17730,#17731,#17732,#17733,#17734,#17735,#17736,#17737,#17738,#17739,#17740,
#17741,#17742,#17743,#17744,#17745,#17746,#17747,#17748,#17749,#17750,#17751,
#17752,#17753,#17754,#17755,#17756,#17757,#17758,#17759,#17760,#17761,#17762,
#17763,#17764,#17765,#17766,#17767,#17768,#17769,#17770,#17771,#17772,#17773,
#17774,#17775,#17776,#17777,#17778,#17779),.UNSPECIFIED.,.F.,.F.,(4,3,3,
3,3,3,3,3,3,3,3,3,3,3,3,3,3,3,3,3,3,3,3,3,3,3,3,3,3,3,3,3,3,3,3,3,3,3,3,
3,3,3,3,3,3,3,3,3,3,3,3,3,3,3,3,3,3,3,3,3,3,3,4),(40.8407044968192,40.951482526017,
41.0639840497603,41.1082697494789,41.1982356380105,41.2880874111166,41.3778496006144,
41.4675490798005,41.5572154228913,41.6468706797942,41.7365368864571,41.8262924173454,
41.9160921411777,42.0060378143554,42.0913764370014,42.1813404376952,42.2711903224086,
42.360950625365,42.450648228453,42.5403127024289,42.6299660993487,42.7196304573156,
42.8093841686622,42.8991820861551,42.9891259945089,43.0744831245238,43.1644485683026,
43.2542998832628,43.3440616019953,43.4337605934291,43.5234264386267,43.6130811881496,
43.7027468785928,43.7925018826807,43.8823010731662,43.9722462076546,44.0575898120463,
44.1475598558189,44.2374158021611,44.3271821773257,44.4168858437695,44.5065563736366,
44.5962158119131,44.6858861896211,44.7756458494045,44.8654496852523,44.9553993981455,
45.0406964995687,45.1306501229485,45.2204896313972,45.3102395722759,45.3999268766119,
45.4895810937788,45.5792242875719,45.6688785078763,45.7586222469766,45.8484102676146,
45.9383445117658,46.0238031870912,46.1137612809231,46.2036191334627,46.2933813462544,
46.3346777312564),.UNSPECIFIED.);
#1242=B_SPLINE_CURVE_WITH_KNOTS('',3,(#17783,#17784,#17785,#17786,#17787,
#17788,#17789,#17790,#17791,#17792,#17793,#17794,#17795,#17796,#17797,#17798,
#17799,#17800,#17801,#17802,#17803,#17804,#17805,#17806,#17807,#17808,#17809,
#17810,#17811,#17812,#17813,#17814,#17815,#17816,#17817,#17818,#17819,#17820,
#17821,#17822,#17823,#17824,#17825,#17826,#17827,#17828,#17829,#17830,#17831,
#17832,#17833,#17834,#17835,#17836,#17837,#17838,#17839,#17840,#17841,#17842,
#17843,#17844,#17845,#17846,#17847,#17848,#17849,#17850,#17851,#17852,#17853,
#17854,#17855,#17856,#17857,#17858),.UNSPECIFIED.,.F.,.F.,(4,3,3,3,3,3,
3,3,3,3,3,3,3,3,3,3,3,3,3,3,3,3,3,3,3,4),(-4.09289414414334,-3.95955978524779,
-3.93242675008978,-3.84608852572687,-3.75985370563718,-3.67370105299863,
-3.58315342919472,-3.49709435009809,-3.41104793156076,-3.32499509288074,
-3.2389167535879,-3.15274805448362,-3.06652690774132,-2.98018641192965,
-2.94932006256734,-2.86503523867605,-2.7808550431761,-2.69675631414078,
-2.61271378948831,-2.52869995275755,-2.44469404013561,-2.36067529736391,
-2.27657679923735,-2.1924341240595,-2.10817127163918,-2.0620931210805),
 .UNSPECIFIED.);
#1243=B_SPLINE_CURVE_WITH_KNOTS('',3,(#17862,#17863,#17864,#17865,#17866,
#17867,#17868,#17869,#17870,#17871,#17872,#17873,#17874,#17875,#17876,#17877,
#17878,#17879,#17880,#17881,#17882,#17883,#17884,#17885,#17886,#17887,#17888,
#17889,#17890,#17891,#17892,#17893,#17894,#17895,#17896,#17897,#17898),
 .UNSPECIFIED.,.F.,.F.,(4,3,3,3,3,3,3,3,3,3,3,3,4),(1.81618237516675E-14,
0.097465303689673,0.19598731370756,0.293525795470838,0.39253956961603,0.491553343761223,
0.578514655128871,0.6654680789535,0.752463591152448,0.839480487924647,0.926580031428077,
0.983106687522448,1.10990010696217),.UNSPECIFIED.);
#1244=B_SPLINE_CURVE_WITH_KNOTS('',3,(#17900,#17901,#17902,#17903,#17904,
#17905,#17906,#17907,#17908,#17909,#17910,#17911,#17912,#17913,#17914,#17915,
#17916,#17917,#17918,#17919,#17920,#17921,#17922,#17923,#17924,#17925,#17926,
#17927,#17928,#17929,#17930,#17931,#17932,#17933,#17934,#17935,#17936,#17937,
#17938,#17939,#17940,#17941,#17942,#17943,#17944,#17945,#17946,#17947,#17948,
#17949,#17950,#17951,#17952,#17953,#17954,#17955,#17956,#17957,#17958,#17959,
#17960,#17961,#17962,#17963,#17964,#17965,#17966,#17967,#17968,#17969,#17970,
#17971,#17972,#17973,#17974,#17975,#17976,#17977,#17978,#17979,#17980,#17981,
#17982,#17983,#17984,#17985,#17986,#17987,#17988,#17989,#17990,#17991,#17992,
#17993,#17994,#17995,#17996,#17997,#17998,#17999,#18000,#18001,#18002,#18003,
#18004,#18005,#18006,#18007,#18008,#18009,#18010,#18011,#18012,#18013,#18014,
#18015,#18016,#18017,#18018,#18019,#18020,#18021,#18022,#18023,#18024,#18025,
#18026,#18027,#18028,#18029,#18030,#18031,#18032,#18033,#18034,#18035,#18036,
#18037,#18038,#18039,#18040,#18041,#18042,#18043,#18044,#18045,#18046,#18047,
#18048,#18049,#18050,#18051,#18052,#18053,#18054,#18055,#18056,#18057,#18058,
#18059,#18060,#18061,#18062,#18063,#18064,#18065,#18066,#18067,#18068,#18069,
#18070,#18071,#18072,#18073,#18074,#18075,#18076,#18077,#18078,#18079,#18080,
#18081,#18082,#18083,#18084,#18085,#18086,#18087,#18088,#18089,#18090,#18091,
#18092,#18093,#18094,#18095,#18096,#18097,#18098,#18099,#18100,#18101,#18102,
#18103,#18104,#18105,#18106,#18107,#18108,#18109,#18110,#18111,#18112,#18113,
#18114,#18115,#18116,#18117,#18118,#18119,#18120,#18121,#18122,#18123,#18124,
#18125,#18126,#18127,#18128),.UNSPECIFIED.,.F.,.F.,(4,3,3,3,3,3,3,3,3,3,
3,3,3,3,3,3,3,3,3,3,3,3,3,3,3,3,3,3,3,3,3,3,3,3,3,3,3,3,3,3,3,3,3,3,3,3,
3,3,3,3,3,3,3,3,3,3,3,3,3,3,3,3,3,3,3,3,3,3,3,3,3,3,3,3,3,3,4),(1.10990010708344,
1.1961286058751,1.28229535123711,1.36843172567019,1.4545539136249,1.54068094018495,
1.62683182926768,1.71308212960078,1.79938293490773,1.88582928212476,1.96621337504489,
2.05153108173538,2.13673294970428,2.22184143229054,2.30687888662215,2.3918736400768,
2.47684792459047,2.56182185653531,2.64681554817045,2.73189761684025,2.81702879702236,
2.90228614623796,2.94932006256734,3.03565805991247,3.12189270046458,3.2080452208331,
3.29859291199018,3.38465197828492,3.47069842778444,3.55675134115351,3.64282979885581,
3.72899868109771,3.81522004855201,3.90156081956687,3.93242675008978,4.01862531663163,
4.10472062379942,4.19073408969261,4.27668705919604,4.36260993804403,4.44852003617063,
4.53443659800429,4.62037886781216,4.70641359734286,4.79250118256877,4.87871238538384,
4.91553343761223,5.00156375899611,5.08748769640701,5.17332689219006,5.25910291179368,
5.3448454961129,5.43057326880457,5.51630566495775,5.60206211830088,5.68790953458488,
5.77380869437548,5.85983139642645,5.89864012513467,5.98479447136155,6.07084407042382,
6.15681040430506,6.24271488026911,6.32858741328564,6.41444602624368,6.50031001604005,
6.58619867867155,6.67217852283113,6.75821041676436,6.84436517205843,6.88174681265712,
6.97139414465698,7.06090018627908,7.15023013756892,7.23945576258717,7.32855559990409,
7.39308541414175),.UNSPECIFIED.);
#1245=B_SPLINE_CURVE_WITH_KNOTS('',3,(#18130,#18131,#18132,#18133,#18134,
#18135,#18136,#18137,#18138,#18139,#18140,#18141,#18142,#18143,#18144,#18145,
#18146,#18147,#18148,#18149,#18150,#18151,#18152,#18153,#18154,#18155,#18156,
#18157,#18158,#18159,#18160,#18161,#18162,#18163,#18164,#18165,#18166,#18167,
#18168,#18169,#18170,#18171,#18172,#18173,#18174,#18175,#18176,#18177,#18178,
#18179,#18180,#18181,#18182,#18183,#18184,#18185,#18186,#18187,#18188,#18189,
#18190,#18191,#18192,#18193,#18194,#18195,#18196,#18197,#18198,#18199,#18200,
#18201,#18202,#18203,#18204,#18205,#18206,#18207,#18208,#18209,#18210,#18211,
#18212,#18213,#18214,#18215,#18216,#18217,#18218,#18219,#18220,#18221,#18222,
#18223,#18224,#18225,#18226,#18227,#18228,#18229,#18230,#18231,#18232,#18233,
#18234,#18235,#18236,#18237,#18238,#18239,#18240,#18241,#18242,#18243,#18244,
#18245,#18246,#18247,#18248,#18249,#18250,#18251,#18252,#18253,#18254,#18255,
#18256,#18257,#18258,#18259,#18260,#18261,#18262,#18263,#18264,#18265,#18266,
#18267,#18268,#18269,#18270,#18271,#18272,#18273,#18274,#18275,#18276,#18277,
#18278,#18279,#18280,#18281,#18282,#18283,#18284,#18285,#18286,#18287,#18288,
#18289,#18290,#18291,#18292,#18293,#18294,#18295,#18296,#18297,#18298,#18299,
#18300,#18301,#18302,#18303,#18304,#18305,#18306,#18307,#18308,#18309,#18310,
#18311,#18312,#18313,#18314,#18315,#18316,#18317,#18318,#18319,#18320,#18321,
#18322,#18323,#18324,#18325,#18326,#18327,#18328,#18329,#18330,#18331,#18332,
#18333,#18334,#18335,#18336,#18337,#18338,#18339,#18340,#18341,#18342,#18343,
#18344,#18345,#18346,#18347,#18348,#18349,#18350,#18351,#18352,#18353,#18354,
#18355,#18356,#18357,#18358,#18359,#18360,#18361),.UNSPECIFIED.,.F.,.F.,
(4,3,3,3,3,3,3,3,3,3,3,3,3,3,3,3,3,3,3,3,3,3,3,3,3,3,3,3,3,3,3,3,3,3,3,
3,3,3,3,3,3,3,3,3,3,3,3,3,3,3,3,3,3,3,3,3,3,3,3,3,3,3,3,3,3,3,3,3,3,3,3,
3,3,3,3,3,3,4),(7.3930854143344,7.48366125998094,7.5789593200306,7.66991850903281,
7.7610068757006,7.85228887176144,7.86485350017956,7.95096567356472,8.0369726336412,
8.12289591723387,8.20875698581783,8.29458574146171,8.3804003602425,8.4662201866803,
8.55206456429625,8.63800018005379,8.7239878182005,8.81009865991351,8.84796018770201,
8.93408705165396,9.02010890939336,9.10604727849447,9.19192360144347,9.27776780665372,
9.36359799193743,9.44943348524598,9.53529361359441,9.62124502178279,9.70724849768268,
9.79337510940081,9.83106687522445,9.91718938261793,10.0032068469648,10.0891407914262,
10.1750126640201,10.2608523972262,10.3466780984187,10.4325091004347,10.5183647351718,
10.604311670713,10.6903106799034,10.7764328728798,10.8141735627469,10.9002949112415,
10.9863111869436,11.0722439146069,11.1581145438086,11.2439529984951,11.3297773996506,
11.4156070814413,11.5014613770805,11.5874069521317,11.6734045867373,11.7595253953439,
11.7972802502693,11.8834032732732,11.9694212484686,12.0553556984052,12.1412280704876,
12.2270682923214,12.3128944752081,12.3987259514211,12.4845820522888,12.5705294391601,
12.6565288918185,12.7426515122888,12.7803869377918,12.8655355434748,12.9505796553732,
13.0355418164815,13.1204452668709,13.20531838703,13.2901814231804,13.3750546099121,
13.4600018316116,13.5449901073353,13.6300921524228,13.6762707211195),
 .UNSPECIFIED.);
#1246=B_SPLINE_CURVE_WITH_KNOTS('',3,(#18363,#18364,#18365,#18366,#18367,
#18368,#18369,#18370,#18371,#18372,#18373,#18374,#18375,#18376,#18377,#18378,
#18379,#18380,#18381,#18382,#18383,#18384,#18385,#18386,#18387,#18388,#18389,
#18390,#18391,#18392,#18393,#18394,#18395,#18396,#18397,#18398,#18399,#18400,
#18401,#18402,#18403,#18404,#18405,#18406,#18407,#18408,#18409,#18410,#18411,
#18412,#18413,#18414,#18415,#18416,#18417,#18418,#18419,#18420,#18421,#18422,
#18423,#18424,#18425,#18426,#18427,#18428,#18429,#18430,#18431,#18432,#18433,
#18434,#18435,#18436,#18437,#18438,#18439,#18440,#18441,#18442,#18443,#18444,
#18445,#18446,#18447,#18448,#18449,#18450,#18451,#18452,#18453,#18454,#18455,
#18456,#18457,#18458,#18459,#18460,#18461,#18462,#18463,#18464,#18465,#18466,
#18467,#18468,#18469,#18470,#18471,#18472,#18473,#18474,#18475,#18476,#18477,
#18478,#18479,#18480,#18481,#18482,#18483,#18484,#18485,#18486,#18487,#18488,
#18489,#18490,#18491,#18492,#18493,#18494,#18495,#18496,#18497,#18498,#18499,
#18500,#18501,#18502,#18503,#18504,#18505,#18506,#18507,#18508,#18509,#18510,
#18511,#18512,#18513,#18514,#18515,#18516,#18517,#18518,#18519,#18520,#18521,
#18522,#18523,#18524,#18525,#18526,#18527,#18528,#18529,#18530,#18531,#18532,
#18533,#18534,#18535,#18536,#18537,#18538,#18539,#18540,#18541,#18542,#18543,
#18544,#18545,#18546,#18547,#18548,#18549,#18550,#18551,#18552,#18553,#18554,
#18555,#18556,#18557,#18558,#18559,#18560,#18561,#18562,#18563,#18564,#18565,
#18566,#18567,#18568,#18569,#18570,#18571,#18572,#18573,#18574,#18575,#18576,
#18577,#18578,#18579,#18580,#18581,#18582,#18583,#18584,#18585,#18586,#18587,
#18588,#18589,#18590,#18591),.UNSPECIFIED.,.F.,.F.,(4,3,3,3,3,3,3,3,3,3,
3,3,3,3,3,3,3,3,3,3,3,3,3,3,3,3,3,3,3,3,3,3,3,3,3,3,3,3,3,3,3,3,3,3,3,3,
3,3,3,3,3,3,3,3,3,3,3,3,3,3,3,3,3,3,3,3,3,3,3,3,3,3,3,3,3,3,4),(13.6762707213213,
13.7634936253142,13.8496159580763,13.9356332340953,14.0215669768221,14.1074386345513,
14.1932781340374,14.2791035898167,14.3649343349407,14.4507897015138,14.536736353218,
14.6227350692125,14.7088569571122,14.7466003128367,14.8327228290312,14.9187402913841,
15.0046742231037,15.0905460722461,15.1763857660457,15.2622114178869,15.3480423606136,
15.4338979261233,15.5198447777085,15.6058436943958,15.6919657824959,15.7297070003591,
15.8158294310186,15.9018468068606,15.9877806512044,16.0736524122154,16.1594920170861,
16.2453175795288,16.3311484324836,16.4170039079444,16.5029506695495,16.5889494961742,
16.675071494867,16.7128136878816,16.7989361209402,16.8849534990149,16.9708873454232,
17.0567591083282,17.1425987148302,17.2284242787398,17.3142551329948,17.4001106095863,
17.4860573720587,17.5720561994008,17.6581781985741,17.695920375404,17.7820428278235,
17.8680602255835,17.953994091976,18.0398658751388,18.1257055022317,18.2115310869334,
18.2973619621599,18.3832174598805,18.4691642436063,18.555163092302,18.6412851127977,
18.6790270629265,18.7651495041418,18.8511668905623,18.9371007454944,19.0229725170903,
19.1088121325003,19.1946377054507,19.2804685688698,19.3663240547399,19.4522708266136,
19.5382696634402,19.6243916721438,19.6621337504489,19.7659686645438,19.8686725452676,
19.9594558713002),.UNSPECIFIED.);
#1247=B_SPLINE_CURVE_WITH_KNOTS('',3,(#18593,#18594,#18595,#18596,#18597,
#18598,#18599,#18600,#18601,#18602),.UNSPECIFIED.,.F.,.F.,(4,1,1,1,1,1,
1,4),(19.9594560285009,20.6452404379713,21.6283471254938,22.6114538130162,
23.5945605005387,24.5776671880611,25.5607738755836,26.2426413356805),
 .UNSPECIFIED.);
#1248=B_SPLINE_CURVE_WITH_KNOTS('',3,(#18604,#18605,#18606,#18607,#18608,
#18609,#18610,#18611,#18612,#18613,#18614,#18615,#18616,#18617,#18618,#18619,
#18620,#18621,#18622,#18623,#18624,#18625,#18626,#18627,#18628,#18629,#18630,
#18631,#18632,#18633,#18634,#18635,#18636,#18637,#18638,#18639,#18640,#18641,
#18642,#18643,#18644,#18645,#18646,#18647,#18648,#18649,#18650,#18651,#18652,
#18653,#18654,#18655,#18656,#18657,#18658,#18659,#18660,#18661,#18662,#18663,
#18664,#18665,#18666,#18667,#18668,#18669,#18670,#18671,#18672,#18673,#18674,
#18675,#18676,#18677,#18678,#18679,#18680,#18681,#18682,#18683,#18684,#18685,
#18686,#18687,#18688,#18689,#18690,#18691,#18692,#18693,#18694,#18695,#18696,
#18697,#18698,#18699,#18700,#18701,#18702,#18703,#18704,#18705,#18706,#18707,
#18708,#18709,#18710,#18711,#18712,#18713,#18714,#18715,#18716,#18717,#18718,
#18719,#18720,#18721,#18722,#18723,#18724,#18725,#18726,#18727,#18728,#18729,
#18730,#18731,#18732,#18733,#18734,#18735,#18736,#18737,#18738,#18739,#18740,
#18741,#18742,#18743,#18744,#18745,#18746,#18747,#18748,#18749,#18750,#18751,
#18752,#18753,#18754,#18755,#18756,#18757,#18758,#18759,#18760,#18761,#18762,
#18763,#18764,#18765,#18766,#18767,#18768,#18769,#18770,#18771,#18772,#18773,
#18774,#18775,#18776,#18777,#18778,#18779,#18780,#18781,#18782,#18783,#18784,
#18785,#18786,#18787,#18788,#18789,#18790,#18791,#18792,#18793,#18794,#18795,
#18796,#18797,#18798,#18799,#18800,#18801,#18802,#18803,#18804,#18805,#18806,
#18807,#18808,#18809,#18810,#18811,#18812,#18813,#18814,#18815,#18816,#18817,
#18818,#18819,#18820,#18821,#18822,#18823,#18824,#18825,#18826,#18827,#18828,
#18829,#18830,#18831,#18832),.UNSPECIFIED.,.F.,.F.,(4,3,3,3,3,3,3,3,3,3,
3,3,3,3,3,3,3,3,3,3,3,3,3,3,3,3,3,3,3,3,3,3,3,3,3,3,3,3,3,3,3,3,3,3,3,3,
3,3,3,3,3,3,3,3,3,3,3,3,3,3,3,3,3,3,3,3,3,3,3,3,3,3,3,3,3,3,4),(26.242641499509,
26.3446941768379,26.4478838155214,26.543880563106,26.6300030833935,26.7160205490677,
26.8019544833399,26.8878263342683,26.9736660287096,27.0594916804797,27.1453226224228,
27.2311781864362,27.3171250354588,27.4031239489703,27.4892460329838,27.5269872506285,
27.6131095715702,27.6991268379978,27.7850605733534,27.8709322259246,27.9567717235579,
28.0425971795424,28.1284279269293,28.2142832978237,28.3002299569284,28.3862286820944,
28.4723505817956,28.5100939381509,28.5962163393846,28.6822336845469,28.7681674970097,
28.8540392249894,28.9398787952556,29.025704322127,29.111535138587,29.1973905766713,
29.2833372997852,29.3693360872299,29.4554580460383,29.4932006256733,29.5793236759997,
29.6653416733656,29.7512761403407,29.8371485243456,29.9229887504622,30.0088149328743,
30.0946464038566,30.1805024947355,30.2664498645006,30.3524492959591,30.4385718891503,
30.4763073131958,30.5624285594366,30.6484447521662,30.7343774160621,30.8202480006432,
30.9060864392999,30.99191084223,31.0777405435947,31.1635948766145,31.2495405156828,
31.3355382296261,31.4216591403216,31.4594140007182,31.5455366257588,31.6315541855686,
31.7174882033962,31.8033601273273,31.8891998789751,31.9750255781243,32.0608565576179,
32.1467121493448,32.2326590112296,32.3186579291363,32.4047800046536,32.4425206882407,
32.5258266428601),.UNSPECIFIED.);
#1249=B_SPLINE_CURVE_WITH_KNOTS('',3,(#18834,#18835,#18836,#18837,#18838,
#18839,#18840,#18841,#18842,#18843,#18844,#18845,#18846,#18847,#18848,#18849,
#18850,#18851,#18852,#18853,#18854,#18855,#18856,#18857,#18858,#18859,#18860,
#18861,#18862,#18863,#18864,#18865,#18866,#18867,#18868,#18869,#18870,#18871,
#18872,#18873,#18874,#18875,#18876,#18877,#18878,#18879,#18880,#18881,#18882,
#18883,#18884,#18885,#18886,#18887,#18888,#18889,#18890,#18891,#18892,#18893,
#18894,#18895,#18896,#18897,#18898,#18899,#18900,#18901,#18902,#18903,#18904,
#18905,#18906,#18907,#18908,#18909,#18910,#18911,#18912,#18913,#18914,#18915,
#18916,#18917,#18918,#18919,#18920,#18921,#18922,#18923,#18924,#18925,#18926,
#18927,#18928,#18929,#18930,#18931,#18932,#18933,#18934,#18935,#18936,#18937,
#18938,#18939,#18940,#18941,#18942,#18943,#18944,#18945,#18946,#18947,#18948,
#18949,#18950,#18951,#18952,#18953,#18954,#18955,#18956,#18957,#18958,#18959,
#18960,#18961,#18962,#18963,#18964,#18965,#18966,#18967,#18968,#18969,#18970,
#18971,#18972,#18973,#18974,#18975,#18976,#18977,#18978,#18979,#18980,#18981,
#18982,#18983,#18984,#18985,#18986,#18987,#18988,#18989,#18990,#18991,#18992,
#18993,#18994,#18995,#18996,#18997,#18998,#18999,#19000,#19001,#19002,#19003,
#19004,#19005,#19006,#19007,#19008,#19009,#19010,#19011,#19012,#19013,#19014,
#19015,#19016,#19017,#19018,#19019,#19020,#19021,#19022,#19023,#19024,#19025,
#19026,#19027,#19028,#19029,#19030,#19031,#19032,#19033,#19034,#19035,#19036,
#19037,#19038,#19039,#19040,#19041,#19042,#19043,#19044,#19045,#19046,#19047,
#19048,#19049,#19050,#19051,#19052,#19053,#19054,#19055,#19056,#19057,#19058,
#19059,#19060,#19061,#19062,#19063,#19064,#19065),.UNSPECIFIED.,.F.,.F.,
(4,3,3,3,3,3,3,3,3,3,3,3,3,3,3,3,3,3,3,3,3,3,3,3,3,3,3,3,3,3,3,3,3,3,3,
3,3,3,3,3,3,3,3,3,3,3,3,3,3,3,3,3,3,3,3,3,3,3,3,3,3,3,3,3,3,3,3,3,3,3,3,
3,3,3,3,3,3,4),(32.5258266430566,32.6109724346887,32.6960210961378,32.7809951098591,
32.8659214354213,32.9508241749927,33.0357235442058,33.1206397523944,33.2056408545587,
33.2906886895505,33.3758609577714,33.4256273757631,33.5117386977598,33.5977449669701,
33.6836677195876,33.7695284165969,33.8553570387069,33.9411716721801,34.0269916614943,
34.1128363502318,34.1987724988946,34.2847607974944,34.3708724891257,34.4087340632856,
34.4948626039088,34.5808860086697,34.6668257949821,34.7527034050599,34.8385487008752,
34.9243798543078,35.0102161927437,35.0960770425472,35.1820289830922,35.2680328840028,
35.3541597537952,35.391840750808,35.4779957931001,35.564045956927,35.6500127247878,
35.7359175043445,35.8217901462905,35.90764874693,35.9935126031944,36.0794010110302,
36.1653804190781,36.2514117725677,36.3375658326432,36.3749474383305,36.4609709985879,
36.5468894484378,36.6327244251594,36.7184974902785,36.8042390095103,36.8899668929997,
36.9757005755,37.0614594912268,37.1473111312689,37.2332155266954,37.3192449713843,
37.3580541258529,37.4442653932351,37.5303710041113,37.616392385932,37.7023508908437,
37.7882757520974,37.8741856189158,37.9600997363509,38.0460373477549,38.132064110626,
38.2181418243531,38.3043403342073,38.3411608133753,38.4323669275132,38.5265281831132,
38.6173539858577,38.7080464538249,38.7985713335135,38.8090119499132),
 .UNSPECIFIED.);
#1250=B_SPLINE_CURVE_WITH_KNOTS('',3,(#19067,#19068,#19069,#19070,#19071,
#19072,#19073,#19074,#19075,#19076,#19077,#19078,#19079,#19080,#19081,#19082,
#19083,#19084,#19085,#19086,#19087,#19088,#19089,#19090,#19091,#19092,#19093,
#19094,#19095,#19096,#19097,#19098,#19099,#19100,#19101,#19102,#19103,#19104,
#19105,#19106,#19107,#19108,#19109,#19110,#19111,#19112,#19113,#19114,#19115,
#19116,#19117,#19118),.UNSPECIFIED.,.F.,.F.,(4,3,3,3,3,3,3,3,3,3,3,3,3,
3,3,3,3,4),(38.8090119500397,38.8986001599551,38.9882861023177,39.0781574059986,
39.1681251672574,39.2582803096457,39.3242675008978,39.4085522045926,39.4927322947236,
39.5768309331739,39.6608734290088,39.7448872573002,39.8288931818936,39.9129119571121,
39.9970107280833,40.0811536853461,40.1654173637519,40.2123859659494),
 .UNSPECIFIED.);
#1251=B_SPLINE_CURVE_WITH_KNOTS('',3,(#19122,#19123,#19124,#19125),
 .UNSPECIFIED.,.F.,.F.,(4,4),(-42.2735875634651,-41.7920059872209),
 .UNSPECIFIED.);
#1252=B_SPLINE_CURVE_WITH_KNOTS('',3,(#19127,#19128,#19129,#19130,#19131,
#19132,#19133,#19134,#19135,#19136,#19137,#19138,#19139,#19140,#19141,#19142,
#19143,#19144,#19145,#19146,#19147,#19148,#19149,#19150,#19151,#19152,#19153,
#19154,#19155,#19156,#19157,#19158,#19159,#19160,#19161,#19162,#19163,#19164,
#19165,#19166,#19167,#19168,#19169,#19170,#19171,#19172,#19173,#19174,#19175,
#19176,#19177,#19178,#19179,#19180,#19181,#19182,#19183,#19184,#19185,#19186,
#19187,#19188,#19189,#19190,#19191,#19192,#19193,#19194,#19195,#19196,#19197,
#19198,#19199,#19200,#19201,#19202,#19203,#19204,#19205,#19206,#19207,#19208,
#19209,#19210,#19211,#19212,#19213,#19214,#19215,#19216,#19217,#19218,#19219,
#19220,#19221,#19222,#19223,#19224,#19225,#19226,#19227,#19228,#19229,#19230,
#19231,#19232,#19233,#19234,#19235,#19236,#19237,#19238,#19239,#19240,#19241,
#19242,#19243,#19244,#19245,#19246,#19247,#19248,#19249,#19250,#19251,#19252,
#19253,#19254,#19255,#19256,#19257,#19258,#19259,#19260,#19261,#19262,#19263,
#19264,#19265,#19266,#19267,#19268,#19269,#19270,#19271,#19272,#19273,#19274,
#19275,#19276,#19277,#19278,#19279,#19280,#19281,#19282,#19283,#19284,#19285,
#19286,#19287,#19288,#19289,#19290,#19291,#19292,#19293,#19294,#19295,#19296,
#19297,#19298,#19299,#19300,#19301,#19302,#19303,#19304,#19305,#19306,#19307,
#19308,#19309,#19310,#19311,#19312,#19313,#19314,#19315,#19316,#19317,#19318,
#19319,#19320,#19321,#19322,#19323,#19324,#19325,#19326,#19327,#19328,#19329,
#19330,#19331,#19332,#19333,#19334,#19335,#19336,#19337,#19338,#19339,#19340,
#19341,#19342,#19343,#19344,#19345,#19346,#19347,#19348,#19349,#19350,#19351,
#19352,#19353,#19354,#19355,#19356,#19357,#19358,#19359,#19360,#19361),
 .UNSPECIFIED.,.F.,.F.,(4,3,3,3,3,3,3,3,3,3,3,3,3,3,3,3,3,3,3,3,3,3,3,3,
3,3,3,3,3,3,3,3,3,3,3,3,3,3,3,3,3,3,3,3,3,3,3,3,3,3,3,3,3,3,3,3,3,3,3,3,
3,3,3,3,3,3,3,3,3,3,3,3,3,3,3,3,3,3,4),(-41.79200593275,-41.7820342197039,
-41.6950743300943,-41.6081223321859,-41.5211282447415,-41.4341127720792,
-41.3470146427639,-41.2904808759427,-41.20336832383,-41.1163307621064,-41.0293484847566,
-40.9391016977146,-40.852152878242,-40.7651965641577,-40.6782149646209,
-40.5911902746634,-40.5040544223173,-40.4168531658136,-40.329521224308,
-40.3073741884203,-40.2220564467519,-40.1368545416153,-40.0517460197423,
-39.9667085240719,-39.8817137263903,-39.7967393958665,-39.7117654161815,
-39.6267716751265,-39.5416895547738,-39.4565583215444,-39.3713009176492,
-39.3242675008978,-39.2379295253732,-39.1516949070862,-39.0655424093964,
-38.9749947098938,-38.8889356671652,-38.8028892415144,-38.7168363522496,
-38.6307579188814,-38.5445890611926,-38.4583677184446,-38.3720269721772,
-38.3411608133754,-38.2549622066264,-38.1688668587652,-38.0828533517434,
-37.9969003407262,-37.9109774199415,-37.8250672796277,-37.7391506754001,
-37.6532083630363,-37.567173590932,-37.4810859630649,-37.3948747178714,
-37.3580541258529,-37.2720238464053,-37.1860999512967,-37.1002607981332,
-37.0144848214179,-36.9287422802383,-36.8430145508322,-36.7572821980678,
-36.6715257881743,-36.5856784152043,-36.4997792987108,-36.4137566395602,
-36.3749474383305,-36.2899292270807,-36.2050152151128,-36.1179908982539,
-36.0332183657195,-35.9484752386565,-35.8637411740814,-35.7750110506216,
-35.6901947599964,-35.6053351568716,-35.5203766098291,-35.5088206802422),
 .UNSPECIFIED.);
#1253=B_SPLINE_CURVE_WITH_KNOTS('',3,(#19363,#19364,#19365,#19366,#19367,
#19368,#19369,#19370,#19371,#19372,#19373,#19374,#19375,#19376,#19377,#19378,
#19379,#19380,#19381,#19382,#19383,#19384,#19385,#19386,#19387,#19388,#19389,
#19390,#19391,#19392,#19393,#19394,#19395,#19396,#19397,#19398,#19399,#19400,
#19401,#19402,#19403,#19404,#19405,#19406,#19407,#19408,#19409,#19410,#19411,
#19412,#19413,#19414,#19415,#19416,#19417,#19418,#19419,#19420,#19421,#19422,
#19423,#19424,#19425,#19426,#19427,#19428,#19429,#19430,#19431,#19432,#19433,
#19434,#19435,#19436,#19437,#19438,#19439,#19440,#19441,#19442,#19443,#19444,
#19445,#19446,#19447,#19448,#19449,#19450,#19451,#19452,#19453,#19454,#19455,
#19456,#19457,#19458,#19459,#19460,#19461,#19462,#19463,#19464,#19465,#19466,
#19467,#19468,#19469,#19470,#19471,#19472,#19473,#19474,#19475,#19476,#19477,
#19478,#19479,#19480,#19481,#19482,#19483,#19484,#19485,#19486,#19487,#19488,
#19489,#19490,#19491,#19492,#19493,#19494,#19495,#19496,#19497,#19498,#19499,
#19500,#19501,#19502,#19503,#19504,#19505,#19506,#19507,#19508,#19509,#19510,
#19511,#19512,#19513,#19514,#19515,#19516,#19517,#19518,#19519,#19520,#19521,
#19522,#19523,#19524,#19525,#19526,#19527,#19528,#19529,#19530,#19531,#19532,
#19533,#19534,#19535,#19536,#19537,#19538,#19539,#19540,#19541,#19542,#19543,
#19544,#19545,#19546,#19547,#19548,#19549,#19550,#19551,#19552,#19553,#19554,
#19555,#19556,#19557,#19558,#19559,#19560,#19561,#19562,#19563,#19564,#19565,
#19566,#19567,#19568,#19569,#19570,#19571,#19572,#19573,#19574,#19575,#19576,
#19577,#19578,#19579,#19580,#19581,#19582,#19583,#19584,#19585,#19586,#19587,
#19588,#19589,#19590,#19591),.UNSPECIFIED.,.F.,.F.,(4,3,3,3,3,3,3,3,3,3,
3,3,3,3,3,3,3,3,3,3,3,3,3,3,3,3,3,3,3,3,3,3,3,3,3,3,3,3,3,3,3,3,3,3,3,3,
3,3,3,3,3,3,3,3,3,3,3,3,3,3,3,3,3,3,3,3,3,3,3,3,3,3,3,3,3,3,4),(-35.5088206800413,
-35.391840750808,-35.3057134673612,-35.2196910812655,-35.1337520760534,
-35.0478750102457,-34.9620299050909,-34.8761987221089,-34.7903621339832,
-34.7045008142665,-34.6185480744502,-34.5325431848047,-34.4464150450444,
-34.4087340632856,-34.322621901095,-34.2366149523578,-34.1506916802349,
-34.0648306232373,-33.9790018793112,-33.8931872723268,-33.8073674577515,
-33.7215230920524,-33.6355874882297,-33.5495998620446,-33.4634890322309,
-33.4256273757631,-33.3395005067057,-33.2534786438155,-33.1675402695245,
-33.0816639413529,-32.9958197308907,-32.9099895403383,-32.8241540417499,
-32.7382939081162,-32.6523424946626,-32.5663390135018,-32.480212396575,
-32.4425206882407,-32.3563981804201,-32.2703807156258,-32.1844467706973,
-32.0985748976172,-32.0127351638982,-31.9269094621762,-31.8410784596148,
-31.7552228243167,-31.6692758881938,-31.5832768784092,-31.4971546848244,
-31.4594140007183,-31.3732926541172,-31.2872763803364,-31.20134365462,-31.1154730273881,
-31.0296345746987,-30.9438101755565,-30.8579804957934,-30.7721262021939,
-30.6861806291898,-30.6001829966384,-30.514062190079,-30.4763073131958,
-30.3901842891515,-30.3041663129045,-30.2182318619066,-30.1323594887544,
-30.046519265842,-29.9606930818716,-29.8748616045711,-29.7890055026128,
-29.7030581146527,-29.6170586609049,-29.5309360393539,-29.4932006256734,
-29.3853784705262,-29.2791332454367,-29.2256353730422),.UNSPECIFIED.);
#1254=B_SPLINE_CURVE_WITH_KNOTS('',3,(#19593,#19594,#19595,#19596,#19597,
#19598,#19599,#19600,#19601,#19602,#19603,#19604,#19605,#19606,#19607,#19608,
#19609,#19610,#19611,#19612,#19613,#19614,#19615,#19616,#19617,#19618,#19619,
#19620,#19621,#19622,#19623,#19624,#19625,#19626,#19627,#19628,#19629,#19630,
#19631,#19632,#19633,#19634,#19635,#19636,#19637,#19638,#19639,#19640,#19641,
#19642,#19643,#19644,#19645,#19646,#19647,#19648,#19649,#19650,#19651,#19652,
#19653,#19654,#19655,#19656,#19657,#19658,#19659,#19660,#19661,#19662,#19663,
#19664,#19665,#19666,#19667,#19668,#19669,#19670,#19671,#19672,#19673,#19674,
#19675,#19676,#19677,#19678,#19679,#19680,#19681,#19682,#19683,#19684,#19685,
#19686,#19687,#19688,#19689,#19690,#19691,#19692,#19693,#19694,#19695,#19696,
#19697,#19698,#19699,#19700,#19701,#19702,#19703,#19704,#19705,#19706,#19707,
#19708,#19709,#19710,#19711,#19712,#19713,#19714,#19715,#19716,#19717,#19718,
#19719,#19720,#19721,#19722,#19723,#19724,#19725,#19726,#19727,#19728,#19729,
#19730,#19731,#19732,#19733,#19734,#19735,#19736,#19737,#19738,#19739,#19740,
#19741,#19742,#19743,#19744,#19745,#19746,#19747,#19748,#19749,#19750,#19751,
#19752,#19753,#19754,#19755,#19756,#19757,#19758,#19759,#19760,#19761,#19762,
#19763,#19764,#19765,#19766,#19767,#19768,#19769,#19770,#19771,#19772,#19773,
#19774,#19775,#19776,#19777,#19778,#19779,#19780,#19781,#19782,#19783,#19784,
#19785,#19786,#19787,#19788,#19789,#19790,#19791,#19792,#19793,#19794,#19795,
#19796,#19797,#19798,#19799,#19800,#19801,#19802,#19803,#19804,#19805,#19806,
#19807,#19808,#19809,#19810,#19811,#19812,#19813,#19814,#19815,#19816,#19817,
#19818,#19819,#19820,#19821,#19822,#19823,#19824),.UNSPECIFIED.,.F.,.F.,
(4,3,3,3,3,3,3,3,3,3,3,3,3,3,3,3,3,3,3,3,3,3,3,3,3,3,3,3,3,3,3,3,3,3,3,
3,3,3,3,3,3,3,3,3,3,3,3,3,3,3,3,3,3,3,3,3,3,3,3,3,3,3,3,3,3,3,3,3,3,3,3,
3,3,3,3,3,3,4),(-29.2256353728617,-29.1361926935229,-29.0511260979808,-28.9660762328229,
-28.88102302201,-28.7959463909764,-28.7107799985853,-28.6255612560834,-28.5402214425233,
-28.5100939381509,-28.4239716056522,-28.3379543299007,-28.2520205874456,
-28.1661489299919,-28.0803094307853,-27.9944839752883,-27.9086532304487,
-27.822797864162,-27.7368512127461,-27.6508524970411,-27.5647306094304,
-27.5269872506285,-27.4408647342574,-27.3548472717257,-27.2689133398253,
-27.1830414905009,-27.0972017965172,-27.0113761444908,-26.9255452015783,
-26.8396896358817,-26.7537427841098,-26.6677438672355,-26.5816217789496,
-26.543880563106,-26.4577581324764,-26.3717407566645,-26.2858069123508,
-26.1999351513698,-26.1140955465289,-26.0282699841158,-25.9424391311903,
-25.856583655759,-25.7706368941827,-25.6846380675869,-25.598516068922,-25.5607738755836,
-25.4746514425571,-25.3886340645148,-25.3027002181393,-25.216828455268,
-25.1309888488002,-25.0451632849252,-24.9593324307051,-24.8734769541487,
-24.7875301917118,-24.7015313644052,-24.6154093652677,-24.5776671880611,
-24.4915447356144,-24.4055273378264,-24.3195934714057,-24.2337216882146,
-24.1478820610932,-24.0620564763624,-23.9762256011071,-23.8903701033575,
-23.8044233196025,-23.7184244708774,-23.6323024503526,-23.5945605005387,
-23.5084383448351,-23.4224191446739,-23.3364834599017,-23.2506119149563,
-23.1647805520879,-23.0789734309571,-22.9931527448939,-22.9424500656821),
 .UNSPECIFIED.);
#1255=B_SPLINE_CURVE_WITH_KNOTS('',3,(#19826,#19827,#19828,#19829,#19830,
#19831,#19832,#19833,#19834,#19835,#19836,#19837,#19838,#19839,#19840,#19841,
#19842,#19843,#19844,#19845,#19846,#19847,#19848,#19849,#19850,#19851,#19852,
#19853,#19854,#19855,#19856,#19857,#19858,#19859,#19860,#19861,#19862,#19863,
#19864,#19865,#19866,#19867,#19868,#19869,#19870,#19871,#19872,#19873,#19874,
#19875,#19876,#19877,#19878,#19879,#19880,#19881,#19882,#19883,#19884,#19885,
#19886,#19887,#19888,#19889,#19890,#19891,#19892,#19893,#19894,#19895,#19896,
#19897,#19898,#19899,#19900,#19901,#19902,#19903,#19904,#19905,#19906,#19907,
#19908,#19909,#19910,#19911,#19912,#19913,#19914,#19915,#19916,#19917,#19918,
#19919,#19920,#19921,#19922,#19923,#19924,#19925,#19926,#19927,#19928,#19929,
#19930,#19931,#19932,#19933,#19934,#19935,#19936,#19937,#19938,#19939,#19940,
#19941,#19942,#19943,#19944,#19945,#19946,#19947,#19948,#19949,#19950,#19951,
#19952,#19953,#19954,#19955,#19956,#19957,#19958,#19959,#19960,#19961,#19962,
#19963,#19964,#19965,#19966,#19967,#19968,#19969,#19970,#19971,#19972,#19973,
#19974,#19975,#19976,#19977,#19978,#19979,#19980,#19981,#19982,#19983,#19984,
#19985,#19986,#19987,#19988,#19989,#19990,#19991,#19992,#19993,#19994,#19995,
#19996,#19997,#19998,#19999,#20000,#20001,#20002,#20003,#20004,#20005,#20006,
#20007,#20008,#20009,#20010,#20011,#20012,#20013,#20014,#20015,#20016,#20017,
#20018,#20019,#20020,#20021,#20022,#20023,#20024,#20025,#20026,#20027,#20028,
#20029,#20030,#20031,#20032,#20033,#20034,#20035,#20036,#20037,#20038,#20039,
#20040,#20041,#20042,#20043,#20044,#20045,#20046,#20047,#20048,#20049,#20050,
#20051,#20052,#20053,#20054,#20055,#20056,#20057),.UNSPECIFIED.,.F.,.F.,
(4,3,3,3,3,3,3,3,3,3,3,3,3,3,3,3,3,3,3,3,3,3,3,3,3,3,3,3,3,3,3,3,3,3,3,
3,3,3,3,3,3,3,3,3,3,3,3,3,3,3,3,3,3,3,3,3,3,3,3,3,3,3,3,3,3,3,3,3,3,3,3,
3,3,3,3,3,3,4),(-22.9424500654921,-22.8432492269214,-22.743518032141,-22.6431790088504,
-22.6114538130162,-22.525331370706,-22.4393139831972,-22.3533801271849,
-22.2675083545179,-22.1816687380548,-22.0958431640629,-22.0100122996148,
-21.92415681273,-21.838210039868,-21.7522112020671,-21.6660891924192,-21.6283471254938,
-21.5422246798375,-21.4562072889451,-21.370273429516,-21.2844016534033,
-21.1985620334634,-21.1127364559765,-21.0269055880192,-20.9410500976143,
-20.855103321235,-20.7691044799135,-20.6829824667704,-20.6452404379714,
-20.5591179957949,-20.4731006083946,-20.3871667524656,-20.3012949798572,
-20.215455363415,-20.1296297894206,-20.0437989249469,-19.9579434380131,
-19.8719966650674,-19.7859978271626,-19.6998758173811,-19.6621337504489,
-19.5760113092192,-19.4899939227884,-19.4040600678502,-19.3181882962524,
-19.2323486808462,-19.1465231079036,-19.0606922444959,-18.9748367586413,
-18.8888899867884,-18.8028911499858,-18.716769141311,-18.6790270629265,
-18.5929046099203,-18.5068872116786,-18.4209533449092,-18.3350815614742,
-18.2492419342651,-18.1634163495443,-18.0775854743959,-17.9917299768508,
-17.905783193446,-17.8197843451551,-17.733662325189,-17.695920375404,-17.609797943694,
-17.5237805667203,-17.4378467211662,-17.3519749588694,-17.2661353526079,
-17.18030978871,-17.0944789342378,-17.0086234572,-16.9226766939388,-16.8366778656107,
-16.7505558651585,-16.7128136878816,-16.6592647585025),.UNSPECIFIED.);
#1256=B_SPLINE_CURVE_WITH_KNOTS('',3,(#20059,#20060,#20061,#20062,#20063,
#20064,#20065,#20066,#20067,#20068,#20069,#20070,#20071,#20072,#20073,#20074,
#20075,#20076,#20077,#20078,#20079,#20080,#20081,#20082,#20083,#20084,#20085,
#20086,#20087,#20088,#20089,#20090,#20091,#20092,#20093,#20094,#20095,#20096,
#20097,#20098,#20099,#20100,#20101,#20102,#20103,#20104,#20105,#20106,#20107,
#20108,#20109,#20110,#20111,#20112,#20113,#20114,#20115,#20116,#20117,#20118,
#20119,#20120,#20121,#20122,#20123,#20124,#20125,#20126,#20127,#20128,#20129,
#20130,#20131,#20132,#20133,#20134,#20135,#20136,#20137,#20138,#20139,#20140,
#20141,#20142,#20143,#20144,#20145,#20146,#20147,#20148,#20149,#20150,#20151,
#20152,#20153,#20154,#20155,#20156,#20157,#20158,#20159,#20160,#20161,#20162,
#20163,#20164,#20165,#20166,#20167,#20168,#20169,#20170,#20171,#20172,#20173,
#20174,#20175,#20176,#20177,#20178,#20179,#20180,#20181,#20182,#20183,#20184,
#20185,#20186,#20187,#20188,#20189,#20190,#20191,#20192,#20193,#20194,#20195,
#20196,#20197,#20198,#20199,#20200,#20201,#20202,#20203,#20204,#20205,#20206,
#20207,#20208,#20209,#20210,#20211,#20212,#20213,#20214,#20215,#20216,#20217,
#20218,#20219,#20220,#20221,#20222,#20223,#20224,#20225,#20226,#20227,#20228,
#20229,#20230,#20231,#20232,#20233,#20234,#20235,#20236,#20237,#20238,#20239,
#20240,#20241,#20242,#20243,#20244,#20245,#20246,#20247,#20248,#20249,#20250,
#20251,#20252,#20253,#20254,#20255,#20256,#20257,#20258,#20259,#20260,#20261,
#20262,#20263,#20264,#20265,#20266,#20267,#20268,#20269,#20270,#20271,#20272,
#20273,#20274,#20275,#20276,#20277,#20278,#20279,#20280,#20281,#20282,#20283,
#20284,#20285,#20286,#20287),.UNSPECIFIED.,.F.,.F.,(4,3,3,3,3,3,3,3,3,3,
3,3,3,3,3,3,3,3,3,3,3,3,3,3,3,3,3,3,3,3,3,3,3,3,3,3,3,3,3,3,3,3,3,3,3,3,
3,3,3,3,3,3,3,3,3,3,3,3,3,3,3,3,3,3,3,3,3,3,3,3,3,3,3,3,3,3,4),(-16.6592647583472,
-16.5738430149373,-16.4885227334712,-16.4032816523275,-16.3180945864984,
-16.2329356250115,-16.1477847574117,-16.0626219831902,-15.9773761668429,
-15.8920884458071,-15.8066680671297,-15.7297070003591,-15.6435844798867,
-15.5575670140271,-15.471633079569,-15.3857612284546,-15.2999215338279,
-15.2140958818728,-15.1282649397453,-15.0424093755484,-14.9564625263443,
-14.8704636126523,-14.7843415284612,-14.7466003128367,-14.6604779921827,
-14.5744607260426,-14.4885269909739,-14.4026553386888,-14.3168158413389,
-14.2309903856361,-14.145159638529,-14.0593042679126,-13.9733576090808,
-13.8873588841852,-13.8012369847486,-13.7634936253142,-13.6773712241262,
-13.5913538790123,-13.5054200666001,-13.4195483386733,-13.3337087684636,
-13.2478832416506,-13.162052425251,-13.0761969872289,-12.99025026418,-12.9042514768019,
-12.8181295180617,-12.7803869377918,-12.6942638863894,-12.6082458879433,
-12.5223114198845,-12.4364390347946,-12.3505988075939,-12.2647726240988,
-12.1789411520357,-12.0930850600792,-12.0071376892478,-11.9211382567276,
-11.8350156624911,-11.7972802502693,-11.7111590060667,-11.6251428153763,
-11.5392101535174,-11.4533395709698,-11.367501134333,-11.2816767334135,
-11.195847034049,-11.1099927030158,-11.0240470659038,-10.9380493539021,
-10.851928445109,-10.8141735627469,-10.7213212232863,-10.6287599994176,
-10.5363786705168,-10.4442738471014,-10.3760794514417),.UNSPECIFIED.);
#1257=B_SPLINE_CURVE_WITH_KNOTS('',3,(#20288,#20289,#20290,#20291,#20292,
#20293,#20294,#20295,#20296,#20297,#20298,#20299,#20300,#20301,#20302,#20303,
#20304,#20305,#20306,#20307,#20308,#20309,#20310,#20311,#20312,#20313,#20314,
#20315,#20316,#20317,#20318,#20319,#20320,#20321,#20322,#20323,#20324,#20325,
#20326,#20327,#20328,#20329,#20330,#20331,#20332,#20333,#20334,#20335,#20336,
#20337,#20338,#20339,#20340,#20341,#20342,#20343,#20344,#20345,#20346,#20347,
#20348,#20349,#20350,#20351,#20352,#20353,#20354,#20355,#20356,#20357,#20358,
#20359,#20360,#20361,#20362,#20363,#20364,#20365,#20366,#20367,#20368,#20369,
#20370,#20371,#20372,#20373,#20374,#20375,#20376,#20377,#20378,#20379,#20380,
#20381,#20382,#20383,#20384,#20385,#20386,#20387,#20388,#20389,#20390,#20391,
#20392,#20393,#20394,#20395,#20396,#20397,#20398,#20399,#20400,#20401,#20402,
#20403,#20404,#20405,#20406,#20407,#20408,#20409,#20410,#20411,#20412,#20413,
#20414,#20415,#20416,#20417,#20418,#20419,#20420,#20421,#20422,#20423,#20424,
#20425,#20426,#20427,#20428,#20429,#20430,#20431,#20432,#20433,#20434,#20435,
#20436,#20437,#20438,#20439,#20440,#20441,#20442,#20443,#20444,#20445,#20446,
#20447,#20448,#20449,#20450,#20451,#20452,#20453,#20454,#20455,#20456,#20457,
#20458,#20459,#20460,#20461,#20462,#20463,#20464,#20465,#20466,#20467,#20468,
#20469,#20470,#20471,#20472,#20473,#20474,#20475,#20476,#20477,#20478,#20479,
#20480,#20481,#20482,#20483,#20484,#20485,#20486,#20487,#20488,#20489,#20490,
#20491,#20492,#20493,#20494,#20495,#20496,#20497,#20498,#20499,#20500,#20501,
#20502,#20503,#20504,#20505,#20506,#20507,#20508,#20509,#20510,#20511,#20512,
#20513,#20514,#20515,#20516,#20517,#20518,#20519),.UNSPECIFIED.,.F.,.F.,
(4,3,3,3,3,3,3,3,3,3,3,3,3,3,3,3,3,3,3,3,3,3,3,3,3,3,3,3,3,3,3,3,3,3,3,
3,3,3,3,3,3,3,3,3,3,3,3,3,3,3,3,3,3,3,3,3,3,3,3,3,3,3,3,3,3,3,3,3,3,3,3,
3,3,3,3,3,3,4),(-10.3760794513229,-10.2880145295059,-10.1998923966073,-10.1076860162616,
-10.0193432467952,-9.93091491142239,-9.84233871959151,-9.83106687522445,
-9.74493984606962,-9.65891785327206,-9.57297937914544,-9.48710298111784,
-9.40125874556535,-9.31542855780065,-9.22959308987034,-9.14373301477612,
-9.05778170156634,-8.97177834463815,-8.88565188756136,-8.84796018770201,
-8.76184887755315,-8.67584262021201,-8.58991987947197,-8.50405919433414,
-8.41823058404444,-8.33241596235659,-8.24659598478001,-8.16075130772062,
-8.07481517058394,-7.98882688343906,-7.90271520305529,-7.86485350017956,
-7.77872495169094,-7.69270153910995,-7.60676174503123,-7.52088412724879,
-7.4350388238479,-7.34920766290605,-7.26337131704426,-7.17751045990625,
-7.09155851220294,-7.00555460422482,-6.91942772756424,-6.88174681265712,
-6.79559175471683,-6.70954157508135,-6.62357479127157,-6.53766999564482,
-6.45179733750838,-6.36593872060825,-6.2800748480303,-6.19418642384597,
-6.10820699948371,-6.02217562967714,-5.936021553422,-5.89864012513467,-5.8126166075868,
-5.72669820066755,-5.64086326704925,-5.55509024515823,-5.46934876919013,
-5.38362092897648,-5.2978872897214,-5.21212841716633,-5.12627681995917,
-5.04037246723583,-4.95434306467912,-4.91553343761223,-4.83052634717772,
-4.74562463000397,-4.66081596132364,-4.57605895127486,-4.49133320716937,
-4.40661836557381,-4.32185837814588,-4.23707535482957,-4.15219887483577,
-4.09289414427482),.UNSPECIFIED.);
#1258=B_SPLINE_CURVE_WITH_KNOTS('',3,(#20522,#20523,#20524,#20525,#20526,
#20527,#20528,#20529,#20530,#20531,#20532,#20533,#20534,#20535,#20536,#20537,
#20538,#20539,#20540,#20541,#20542,#20543,#20544,#20545,#20546,#20547,#20548,
#20549),.UNSPECIFIED.,.F.,.F.,(4,3,3,3,3,3,3,3,3,4),(46.3346777312564,46.4243645657982,
46.5140283060791,46.6036909880087,46.6933746409546,46.7831528323428,46.8729842216755,
46.9629495988034,47.0069098746136,47.1238898038469),.UNSPECIFIED.);
#1259=B_SPLINE_CURVE_WITH_KNOTS('',3,(#20551,#20552,#20553,#20554,#20555,
#20556,#20557,#20558,#20559,#20560,#20561,#20562,#20563,#20564,#20565,#20566,
#20567,#20568,#20569,#20570,#20571,#20572,#20573,#20574,#20575,#20576,#20577,
#20578,#20579,#20580,#20581,#20582,#20583,#20584,#20585,#20586,#20587,#20588,
#20589,#20590,#20591,#20592,#20593,#20594,#20595,#20596,#20597,#20598,#20599,
#20600,#20601,#20602,#20603,#20604,#20605,#20606,#20607,#20608,#20609,#20610,
#20611,#20612,#20613,#20614,#20615,#20616,#20617,#20618,#20619,#20620,#20621,
#20622,#20623,#20624,#20625,#20626,#20627,#20628,#20629,#20630,#20631,#20632,
#20633,#20634,#20635,#20636,#20637,#20638,#20639,#20640,#20641,#20642,#20643,
#20644,#20645,#20646,#20647,#20648,#20649,#20650,#20651,#20652,#20653,#20654,
#20655,#20656,#20657,#20658,#20659,#20660,#20661,#20662,#20663,#20664,#20665,
#20666,#20667,#20668,#20669,#20670,#20671,#20672,#20673,#20674,#20675,#20676,
#20677,#20678,#20679,#20680,#20681,#20682,#20683,#20684,#20685,#20686,#20687,
#20688,#20689,#20690,#20691,#20692,#20693,#20694,#20695,#20696,#20697,#20698,
#20699,#20700,#20701,#20702,#20703,#20704,#20705,#20706,#20707,#20708,#20709,
#20710),.UNSPECIFIED.,.F.,.F.,(4,3,3,3,3,3,3,3,3,3,3,3,3,3,3,3,3,3,3,3,
3,3,3,3,3,3,3,3,3,3,3,3,3,3,3,3,3,3,3,3,3,3,3,3,3,3,3,3,3,3,3,3,3,4),(47.1238898040851,
47.212634310815,47.3012804954036,47.3898536706167,47.4783881657889,47.5669071783758,
47.6554338879542,47.7440444285322,47.8326984185048,47.9214901286793,47.9900165621361,
48.079878475582,48.1696262134622,48.2592844383872,48.3488804771275,48.4384437308739,
48.5279963661167,48.6175605357571,48.707215576596,48.7969155021056,48.8867636103351,
48.9731232496585,49.0631813344679,49.1531246430108,49.2429775986181,49.3327663197129,
49.4225209467818,49.5122634308969,49.6020157083635,49.6918549669428,49.7817372622351,
49.8717626820065,49.956229937181,50.0464205997571,50.1364989391249,50.2264891614412,
50.3164179156243,50.4063141963529,50.4961997669363,50.5860963769902,50.6760809951302,
50.766109414171,50.8562806870504,50.9393366247034,51.0273822113533,51.1153142003882,
51.2043285952813,51.2921153635596,51.379874703757,51.4676302816496,51.5575800511205,
51.6454454055357,51.7364373825343,51.8274293595329),.UNSPECIFIED.);
#1260=B_SPLINE_CURVE_WITH_KNOTS('',3,(#20714,#20715,#20716,#20717,#20718,
#20719,#20720,#20721,#20722,#20723,#20724,#20725,#20726,#20727,#20728,#20729,
#20730,#20731,#20732,#20733,#20734,#20735,#20736,#20737,#20738,#20739,#20740,
#20741,#20742,#20743,#20744,#20745,#20746,#20747,#20748,#20749,#20750,#20751,
#20752,#20753,#20754,#20755,#20756,#20757,#20758,#20759,#20760,#20761,#20762,
#20763,#20764,#20765,#20766,#20767,#20768,#20769,#20770,#20771,#20772,#20773,
#20774,#20775,#20776,#20777,#20778,#20779,#20780,#20781,#20782,#20783,#20784,
#20785,#20786,#20787,#20788,#20789,#20790,#20791,#20792,#20793,#20794,#20795,
#20796,#20797,#20798,#20799,#20800,#20801,#20802,#20803,#20804,#20805,#20806,
#20807,#20808,#20809,#20810,#20811,#20812,#20813,#20814,#20815,#20816,#20817,
#20818,#20819,#20820,#20821,#20822,#20823,#20824,#20825,#20826,#20827,#20828,
#20829,#20830,#20831),.UNSPECIFIED.,.F.,.F.,(4,3,3,3,3,3,3,3,3,3,3,3,3,
3,3,3,3,3,3,3,3,3,3,3,3,3,3,3,3,3,3,3,3,3,3,3,3,3,3,4),(47.1238898038469,
47.2174754673338,47.3111680100548,47.4050579725487,47.4990543518043,47.5932435711771,
47.639145354705,47.7282111079036,47.8171624892304,47.9060250358962,47.9955534116876,
48.0843273344302,48.1730941115943,48.2618766705276,48.3519705134526,48.4409057141138,
48.5315788781706,48.6222520422274,48.7134731108222,48.8045685913688,48.8955611216527,
48.9864649966019,49.0773190413066,49.1681435703031,49.2589588697564,49.3498243415436,
49.4407136971665,49.5317037438762,49.6053587297499,49.69634898757,49.7872668551369,
49.8781345589675,49.9689726175072,50.0598150491269,50.0969120735111,50.1985524169299,
50.3004232260078,50.4023379611143,50.5041923151378,50.5884654172723),
 .UNSPECIFIED.);
#1261=B_SPLINE_CURVE_WITH_KNOTS('',3,(#20832,#20833,#20834,#20835,#20836,
#20837,#20838,#20839,#20840,#20841,#20842,#20843,#20844,#20845,#20846,#20847,
#20848,#20849,#20850,#20851,#20852,#20853),.UNSPECIFIED.,.F.,.F.,(4,2,2,
2,2,2,2,2,2,2,4),(-4.68690655991433,-4.676968004902,-4.66334057591782,-4.57050127017845,
-4.54307441119981,-4.52441781843419,-4.51528697313272,-4.50756272912277,
-4.49611705684078,-4.45806694667936,-4.39249448366002),.UNSPECIFIED.);
#1262=B_SPLINE_CURVE_WITH_KNOTS('',3,(#20880,#20881,#20882,#20883,#20884,
#20885,#20886,#20887,#20888,#20889,#20890,#20891,#20892,#20893,#20894,#20895,
#20896,#20897,#20898,#20899,#20900,#20901,#20902,#20903,#20904,#20905,#20906,
#20907,#20908,#20909,#20910,#20911,#20912,#20913,#20914,#20915,#20916,#20917,
#20918,#20919,#20920,#20921,#20922,#20923,#20924,#20925,#20926,#20927,#20928,
#20929,#20930,#20931,#20932,#20933,#20934,#20935,#20936,#20937,#20938,#20939,
#20940,#20941,#20942,#20943,#20944,#20945,#20946,#20947,#20948,#20949,#20950,
#20951,#20952,#20953,#20954,#20955,#20956,#20957,#20958,#20959,#20960,#20961,
#20962,#20963,#20964,#20965,#20966,#20967),.UNSPECIFIED.,.F.,.F.,(4,3,3,
3,3,3,3,3,3,3,3,3,3,3,3,3,3,3,3,3,3,3,3,3,3,3,3,3,3,4),(2.05878368674717E-14,
0.023405447201913,0.0471352136112047,0.0707669153637672,0.0840367480408261,
0.0878713467795278,0.110975706691734,0.133712282270125,0.150709160734639,
0.158060268187143,0.163470733062873,0.167953178850733,0.189907599318317,
0.201793217244577,0.224252520133955,0.234752288110081,0.240507487537732,
0.24411168274315,0.265861093328888,0.287518743439702,0.309003455419039,
0.317294467212432,0.321188873214287,0.341934990903991,0.362478952452641,
0.367608141617428,0.372096895882347,0.385217611626515,0.405963257762497,
0.415993328865176),.UNSPECIFIED.);
#1263=B_SPLINE_CURVE_WITH_KNOTS('',3,(#20969,#20970,#20971,#20972),
 .UNSPECIFIED.,.F.,.F.,(4,4),(-2.84914982550175,-2.06894047480313),
 .UNSPECIFIED.);
#1264=B_SPLINE_CURVE_WITH_KNOTS('',3,(#20974,#20975,#20976,#20977,#20978,
#20979,#20980,#20981,#20982,#20983,#20984,#20985,#20986,#20987,#20988,#20989,
#20990,#20991,#20992,#20993,#20994,#20995,#20996,#20997,#20998,#20999,#21000,
#21001,#21002,#21003,#21004,#21005,#21006,#21007,#21008,#21009,#21010,#21011,
#21012,#21013,#21014,#21015,#21016,#21017,#21018,#21019,#21020,#21021,#21022,
#21023,#21024,#21025,#21026,#21027,#21028,#21029,#21030,#21031,#21032,#21033,
#21034,#21035,#21036,#21037,#21038,#21039,#21040,#21041,#21042,#21043,#21044,
#21045,#21046,#21047,#21048,#21049,#21050,#21051,#21052,#21053,#21054,#21055,
#21056,#21057,#21058,#21059,#21060,#21061),.UNSPECIFIED.,.F.,.F.,(4,3,3,
3,3,3,3,3,3,3,3,3,3,3,3,3,3,3,3,3,3,3,3,3,3,3,3,3,3,4),(-0.413490722097494,
-0.390374461965417,-0.376956788739721,-0.364612854506389,-0.357223081629536,
-0.353167632297454,-0.329816475307035,-0.3110173587975,-0.300922997939596,
-0.297410089408388,-0.274622870922315,-0.252197899215606,-0.232987043189295,
-0.22435563742345,-0.220563464855743,-0.216970640358496,-0.195389510663287,
-0.179453841006409,-0.157360826323377,-0.146597972574468,-0.141428288189789,
-0.120042549964023,-0.0987340253119133,-0.0775979223516053,-0.0725581786302476,
-0.0680299217253234,-0.0474532857852412,-0.0272139184783649,-0.00761976281229705,
0.),.UNSPECIFIED.);
#1265=B_SPLINE_CURVE_WITH_KNOTS('',3,(#21062,#21063,#21064,#21065,#21066,
#21067,#21068,#21069,#21070,#21071,#21072,#21073,#21074,#21075,#21076,#21077,
#21078,#21079,#21080,#21081,#21082,#21083,#21084,#21085,#21086),
 .UNSPECIFIED.,.F.,.F.,(4,3,3,3,3,3,3,3,4),(16.7019922841306,16.810649070825,
16.9192297222185,17.0277712030643,17.1410987082733,17.2497327354331,17.3584254886797,
17.467270185633,17.4810812239006),.UNSPECIFIED.);
#1266=B_SPLINE_CURVE_WITH_KNOTS('',3,(#21092,#21093,#21094,#21095,#21096,
#21097,#21098,#21099,#21100,#21101,#21102,#21103,#21104,#21105,#21106,#21107,
#21108,#21109,#21110,#21111,#21112,#21113,#21114,#21115,#21116),
 .UNSPECIFIED.,.F.,.F.,(4,3,3,3,3,3,3,3,4),(15.4643166016706,15.573136451511,
15.6818269380766,15.7904251770487,15.9036702413563,16.0122290128815,16.1208010500588,
16.2294623722504,16.2434054342788),.UNSPECIFIED.);
#1267=B_SPLINE_CURVE_WITH_KNOTS('',3,(#21142,#21143,#21144,#21145,#21146,
#21147,#21148,#21149,#21150,#21151,#21152,#21153,#21154,#21155,#21156,#21157,
#21158,#21159,#21160,#21161,#21162,#21163,#21164,#21165,#21166,#21167,#21168,
#21169,#21170,#21171,#21172,#21173,#21174,#21175,#21176,#21177,#21178,#21179,
#21180,#21181,#21182,#21183,#21184,#21185,#21186,#21187,#21188,#21189,#21190,
#21191,#21192,#21193,#21194,#21195,#21196,#21197,#21198,#21199,#21200,#21201,
#21202,#21203,#21204,#21205,#21206,#21207,#21208,#21209,#21210,#21211,#21212,
#21213,#21214,#21215,#21216,#21217,#21218,#21219,#21220,#21221,#21222,#21223,
#21224,#21225,#21226,#21227,#21228,#21229),.UNSPECIFIED.,.F.,.F.,(4,3,3,
3,3,3,3,3,3,3,3,3,3,3,3,3,3,3,3,3,3,3,3,3,3,3,3,3,3,4),(9.94883000103285E-15,
0.019616691656509,0.0399302769755012,0.0573080150775109,0.0651965825194071,
0.0692472851263457,0.0727586240116996,0.0938674469417637,0.115267103019471,
0.136627386511764,0.139448576973331,0.143452860461702,0.147424687779491,
0.169517815215389,0.179453841006421,0.200870095742099,0.220290031668888,
0.22390552179017,0.245971799155713,0.268703017816031,0.291434236476348,
0.297317452472671,0.303372200521482,0.326746258431751,0.349433290040221,
0.355210854434181,0.359640172217466,0.37695678873974,0.400080606868808,
0.414094136780462),.UNSPECIFIED.);
#1268=B_SPLINE_CURVE_WITH_KNOTS('',3,(#21231,#21232,#21233,#21234,#21235,
#21236,#21237,#21238,#21239,#21240,#21241,#21242,#21243,#21244,#21245,#21246,
#21247,#21248,#21249,#21250,#21251,#21252,#21253,#21254,#21255,#21256,#21257,
#21258,#21259,#21260,#21261,#21262,#21263,#21264,#21265,#21266,#21267,#21268,
#21269,#21270,#21271,#21272,#21273,#21274,#21275,#21276,#21277,#21278,#21279,
#21280,#21281,#21282,#21283,#21284,#21285,#21286,#21287,#21288,#21289,#21290,
#21291,#21292,#21293,#21294,#21295,#21296,#21297,#21298,#21299,#21300,#21301,
#21302,#21303,#21304,#21305,#21306,#21307,#21308,#21309,#21310,#21311,#21312,
#21313,#21314,#21315),.UNSPECIFIED.,.F.,.F.,(4,3,3,3,3,3,3,3,3,3,3,3,3,
3,3,3,3,3,3,3,3,3,3,3,3,3,3,3,4),(-0.415993328865187,-0.395247681143785,
-0.385217611626505,-0.373753586977634,-0.368797025934534,-0.36502116844561,
-0.344384137829435,-0.326531494809057,-0.320844694700121,-0.315794800692042,
-0.294447216742868,-0.27264031880428,-0.255006113686598,-0.246851849353904,
-0.243114662305886,-0.220650412226406,-0.201793217244566,-0.179843818696151,
-0.168406146924892,-0.164760369659269,-0.142479944942064,-0.11944136986474,
-0.0964027947874157,-0.086570173338417,-0.0816436307916124,-0.0579861482237484,
-0.0343081270358223,-0.0108824362787603,0.),.UNSPECIFIED.);
#1269=B_SPLINE_CURVE_WITH_KNOTS('',3,(#21316,#21317,#21318,#21319),
 .UNSPECIFIED.,.F.,.F.,(4,4),(0.,0.780209350698613),.UNSPECIFIED.);
#1270=B_SPLINE_CURVE_WITH_KNOTS('',3,(#21521,#21522,#21523,#21524,#21525,
#21526,#21527,#21528,#21529,#21530,#21531,#21532,#21533,#21534,#21535,#21536,
#21537,#21538,#21539,#21540,#21541,#21542,#21543,#21544,#21545,#21546,#21547,
#21548,#21549,#21550,#21551,#21552,#21553,#21554,#21555,#21556,#21557,#21558,
#21559,#21560,#21561,#21562,#21563,#21564,#21565,#21566,#21567,#21568,#21569,
#21570,#21571,#21572,#21573,#21574,#21575,#21576,#21577,#21578,#21579,#21580,
#21581,#21582,#21583,#21584,#21585,#21586,#21587,#21588,#21589,#21590,#21591,
#21592,#21593,#21594,#21595,#21596,#21597,#21598,#21599,#21600,#21601,#21602,
#21603,#21604,#21605,#21606,#21607,#21608,#21609,#21610,#21611,#21612,#21613,
#21614,#21615,#21616,#21617,#21618,#21619,#21620,#21621,#21622,#21623,#21624,
#21625,#21626),.UNSPECIFIED.,.F.,.F.,(4,3,3,3,3,3,3,3,3,3,3,3,3,3,3,3,3,
3,3,3,3,3,3,3,3,3,3,3,3,3,3,3,3,3,3,4),(4.87579287875967E-5,0.0396105854411369,
0.0421684740053724,0.082059122742856,0.12338177968178,0.164704436620703,
0.170094771591715,0.175319647983374,0.214784946467228,0.254291541803321,
0.293151938468816,0.325136464664712,0.334844260977463,0.340168266397053,
0.359707602090094,0.397735946899136,0.434801284779746,0.46134294969662,
0.485996360447615,0.493345060083779,0.498524669937982,0.535408882651194,
0.572734961962543,0.609820594328277,0.632520778240444,0.644430130512825,
0.650618647569442,0.655220962152611,0.658570235704578,0.695166161431644,
0.731571524795797,0.744958227452224,0.754067922795179,0.78988127496075,
0.825088562663305,0.847325527525853),.UNSPECIFIED.);
#1271=B_SPLINE_CURVE_WITH_KNOTS('',3,(#21627,#21628,#21629,#21630,#21631,
#21632,#21633,#21634,#21635,#21636,#21637,#21638,#21639,#21640,#21641,#21642,
#21643,#21644,#21645,#21646,#21647,#21648,#21649,#21650,#21651,#21652,#21653,
#21654,#21655,#21656,#21657,#21658,#21659,#21660,#21661,#21662,#21663,#21664,
#21665,#21666,#21667,#21668,#21669,#21670,#21671,#21672,#21673,#21674,#21675,
#21676,#21677,#21678,#21679,#21680,#21681,#21682,#21683,#21684,#21685,#21686,
#21687,#21688,#21689,#21690,#21691,#21692,#21693,#21694,#21695,#21696,#21697,
#21698,#21699,#21700,#21701,#21702,#21703,#21704,#21705,#21706,#21707,#21708,
#21709,#21710,#21711,#21712,#21713,#21714,#21715,#21716,#21717,#21718,#21719,
#21720),.UNSPECIFIED.,.F.,.F.,(4,3,3,3,3,3,3,3,3,3,3,3,3,3,3,3,3,3,3,3,
3,3,3,3,3,3,3,3,3,3,3,4),(-0.847325527525843,-0.811503753623457,-0.776442908990808,
-0.753769402338684,-0.745431135913051,-0.709753628192895,-0.673219987554428,
-0.651138320105864,-0.645616024847356,-0.608466815738069,-0.57090382277613,
-0.533372849367635,-0.505758215660538,-0.497488333365585,-0.491961441323387,
-0.453421092885502,-0.422238544386844,-0.384505330263272,-0.346772116139701,
-0.33539303508032,-0.33016070262821,-0.291919157069796,-0.252839602001601,
-0.215142387780448,-0.175907489429898,-0.170455452500928,-0.160225010582203,
-0.120305086436378,-0.0801631965284521,-0.0402999487969805,-0.00225557790275668,
-8.80689562460376E-15),.UNSPECIFIED.);
#1272=B_SPLINE_CURVE_WITH_KNOTS('',3,(#21913,#21914,#21915,#21916,#21917,
#21918,#21919,#21920,#21921,#21922,#21923,#21924,#21925,#21926,#21927,#21928,
#21929,#21930,#21931,#21932,#21933,#21934,#21935,#21936,#21937,#21938,#21939,
#21940,#21941,#21942,#21943,#21944,#21945,#21946,#21947,#21948,#21949,#21950,
#21951,#21952,#21953,#21954,#21955,#21956,#21957,#21958,#21959,#21960,#21961,
#21962,#21963,#21964,#21965,#21966,#21967,#21968,#21969,#21970,#21971,#21972,
#21973,#21974,#21975,#21976,#21977,#21978,#21979,#21980,#21981,#21982,#21983,
#21984,#21985,#21986,#21987,#21988,#21989,#21990,#21991,#21992,#21993,#21994,
#21995,#21996,#21997,#21998,#21999,#22000,#22001,#22002,#22003,#22004,#22005,
#22006,#22007,#22008,#22009),.UNSPECIFIED.,.F.,.F.,(4,3,3,3,3,3,3,3,3,3,
3,3,3,3,3,3,3,3,3,3,3,3,3,3,3,3,3,3,3,3,3,3,4),(0.,0.0357326537857237,0.0704414344150977,
0.105764244213075,0.14171479622342,0.147192652306303,0.152214352689264,
0.188537300917028,0.225478864831264,0.26267763210979,0.282838324796318,
0.297126845802674,0.304520830993608,0.342575347752296,0.380671971213311,
0.418209942863103,0.423963173602016,0.455960576699411,0.461085295912164,
0.498135375724191,0.536332170206057,0.574942151961225,0.613574806753294,
0.619086816026134,0.624483039944413,0.630147733446615,0.669254131260838,
0.708784888651943,0.727582209613668,0.735557703752757,0.775673392238865,
0.815702463256823,0.844212290556702),.UNSPECIFIED.);
#1273=B_SPLINE_CURVE_WITH_KNOTS('',3,(#22010,#22011,#22012,#22013,#22014,
#22015,#22016,#22017,#22018,#22019,#22020,#22021,#22022,#22023,#22024,#22025,
#22026,#22027,#22028,#22029,#22030,#22031,#22032,#22033,#22034,#22035,#22036,
#22037,#22038,#22039,#22040,#22041,#22042,#22043,#22044,#22045,#22046,#22047,
#22048,#22049,#22050,#22051,#22052,#22053,#22054,#22055,#22056,#22057,#22058,
#22059,#22060,#22061,#22062,#22063,#22064,#22065,#22066,#22067,#22068,#22069,
#22070,#22071,#22072,#22073,#22074,#22075,#22076,#22077,#22078,#22079,#22080,
#22081,#22082,#22083,#22084,#22085,#22086,#22087,#22088,#22089,#22090,#22091,
#22092,#22093,#22094,#22095,#22096,#22097,#22098,#22099,#22100,#22101,#22102,
#22103,#22104,#22105,#22106,#22107,#22108,#22109),.UNSPECIFIED.,.F.,.F.,
(4,3,3,3,3,3,3,3,3,3,3,3,3,3,3,3,3,3,3,3,3,3,3,3,3,3,3,3,3,3,3,3,3,4),(-0.844212290556731,
-0.804914039435832,-0.802217933301225,-0.761983565707593,-0.738497702142073,
-0.731371284183562,-0.724667747997382,-0.685031612027754,-0.645191108329531,
-0.631145243959577,-0.622466655133243,-0.614790169492861,-0.575459911227575,
-0.536634531463482,-0.497051833947599,-0.459723508709767,-0.457469136431715,
-0.452285602603943,-0.414914580183337,-0.385002433230672,-0.347227915621759,
-0.309590191025686,-0.301425288615579,-0.295199281958322,-0.258388869024602,
-0.221724085233776,-0.188385367654945,-0.153950864306229,-0.147824231453246,
-0.142510002622108,-0.106551008289361,-0.0707579690404533,-0.0353789845202334,
-1.35445026026053E-14),.UNSPECIFIED.);
#1274=B_SPLINE_CURVE_WITH_KNOTS('',3,(#22157,#22158,#22159,#22160,#22161,
#22162,#22163,#22164),.UNSPECIFIED.,.F.,.F.,(4,2,2,4),(0.,0.000697892015497008,
0.0143255677369775,0.0286350340362092),.UNSPECIFIED.);
#1275=B_SPLINE_CURVE_WITH_KNOTS('',3,(#22168,#22169,#22170,#22171,#22172,
#22173),.UNSPECIFIED.,.F.,.F.,(4,2,4),(0.,0.0523373446002982,0.104355593610831),
 .UNSPECIFIED.);
#1276=B_SPLINE_CURVE_WITH_KNOTS('',3,(#22177,#22178,#22179,#22180,#22181,
#22182,#22183,#22184),.UNSPECIFIED.,.F.,.F.,(4,2,2,4),(0.,0.00526521584710592,
0.0639602373511304,0.128212067318051),.UNSPECIFIED.);
#1277=B_SPLINE_CURVE_WITH_KNOTS('',3,(#22188,#22189,#22190,#22191,#22192,
#22193,#22194,#22195),.UNSPECIFIED.,.F.,.F.,(4,2,2,4),(0.,0.0627475271162915,
0.120075061733582,0.125236068694296),.UNSPECIFIED.);
#1278=B_SPLINE_CURVE_WITH_KNOTS('',3,(#22199,#22200,#22201,#22202,#22203,
#22204,#22205,#22206),.UNSPECIFIED.,.F.,.F.,(4,2,2,4),(0.,0.00526560282662867,
0.0639612078258487,0.128213120660444),.UNSPECIFIED.);
#1279=B_SPLINE_CURVE_WITH_KNOTS('',3,(#22210,#22211,#22212,#22213,#22214,
#22215,#22216,#22217),.UNSPECIFIED.,.F.,.F.,(4,2,2,4),(0.,0.0627475590562519,
0.120075649624267,0.125237044527633),.UNSPECIFIED.);
#1280=B_SPLINE_CURVE_WITH_KNOTS('',3,(#22221,#22222,#22223,#22224,#22225,
#22226,#22227,#22228),.UNSPECIFIED.,.F.,.F.,(4,2,2,4),(0.,0.00526602648868038,
0.0639622680416072,0.128214273235454),.UNSPECIFIED.);
#1281=B_SPLINE_CURVE_WITH_KNOTS('',3,(#22232,#22233,#22234,#22235,#22236,
#22237,#22238,#22239),.UNSPECIFIED.,.F.,.F.,(4,2,2,4),(0.,0.0627475953399776,
0.120076292215752,0.125238111923284),.UNSPECIFIED.);
#1282=B_SPLINE_CURVE_WITH_KNOTS('',3,(#22243,#22244,#22245,#22246,#22247,
#22248,#22249,#22250),.UNSPECIFIED.,.F.,.F.,(4,2,2,4),(0.,0.00526649276184272,
0.0639634322919596,0.128215541011568),.UNSPECIFIED.);
#1283=B_SPLINE_CURVE_WITH_KNOTS('',3,(#22254,#22255,#22256,#22257,#22258,
#22259,#22260,#22261),.UNSPECIFIED.,.F.,.F.,(4,2,2,4),(0.,0.0627476367935851,
0.120076998293466,0.125239285656593),.UNSPECIFIED.);
#1284=B_SPLINE_CURVE_WITH_KNOTS('',3,(#22265,#22266,#22267,#22268,#22269,
#22270,#22271,#22272),.UNSPECIFIED.,.F.,.F.,(4,2,2,4),(0.,0.00526700898296905,
0.0639647182192301,0.128216943693669),.UNSPECIFIED.);
#1285=B_SPLINE_CURVE_WITH_KNOTS('',3,(#22276,#22277,#22278,#22279,#22280,
#22281,#22282,#22283),.UNSPECIFIED.,.F.,.F.,(4,2,2,4),(0.,0.0627476844547414,
0.120077778736361,0.125240584036134),.UNSPECIFIED.);
#1286=B_SPLINE_CURVE_WITH_KNOTS('',3,(#22287,#22288,#22289,#22290,#22291,
#22292,#22293,#22294),.UNSPECIFIED.,.F.,.F.,(4,2,2,4),(0.,0.0052675843601308,
0.0639661480124282,0.12821850616927),.UNSPECIFIED.);
#1287=B_SPLINE_CURVE_WITH_KNOTS('',3,(#22298,#22299,#22300,#22301,#22302,
#22303,#22304,#22305),.UNSPECIFIED.,.F.,.F.,(4,2,2,4),(0.,0.0627497316200279,
0.120007641766305,0.125309768916132),.UNSPECIFIED.);
#1288=B_SPLINE_CURVE_WITH_KNOTS('',3,(#22311,#22312,#22313,#22314,#22315,
#22316),.UNSPECIFIED.,.F.,.F.,(4,2,4),(1.75570920373614E-15,0.0320055376006011,
0.0638199285984987),.UNSPECIFIED.);
#1289=B_SPLINE_CURVE_WITH_KNOTS('',3,(#22320,#22321,#22322,#22323,#22324,
#22325,#22326,#22327),.UNSPECIFIED.,.F.,.F.,(4,2,2,4),(0.,0.00526977567755582,
0.0639683005470083,0.128217977351555),.UNSPECIFIED.);
#1290=B_SPLINE_CURVE_WITH_KNOTS('',3,(#22331,#22332,#22333,#22334,#22335,
#22336,#22337,#22338),.UNSPECIFIED.,.F.,.F.,(4,2,2,4),(0.,0.062761494454614,
0.120090502459536,0.125241025317951),.UNSPECIFIED.);
#1291=B_SPLINE_CURVE_WITH_KNOTS('',3,(#22342,#22343,#22344,#22345,#22346,
#22347,#22348,#22349),.UNSPECIFIED.,.F.,.F.,(4,2,2,4),(0.,0.00526922229267531,
0.0639669243235216,0.128216474527037),.UNSPECIFIED.);
#1292=B_SPLINE_CURVE_WITH_KNOTS('',3,(#22353,#22354,#22355,#22356,#22357,
#22358,#22359,#22360),.UNSPECIFIED.,.F.,.F.,(4,2,2,4),(0.,0.0627614441556716,
0.120089692527127,0.125239677665907),.UNSPECIFIED.);
#1293=B_SPLINE_CURVE_WITH_KNOTS('',3,(#22364,#22365,#22366,#22367,#22368,
#22369,#22370,#22371),.UNSPECIFIED.,.F.,.F.,(4,2,2,4),(0.,0.0052687245725873,
0.0639656835644766,0.128215122077758),.UNSPECIFIED.);
#1294=B_SPLINE_CURVE_WITH_KNOTS('',3,(#22375,#22376,#22377,#22378,#22379,
#22380,#22381,#22382),.UNSPECIFIED.,.F.,.F.,(4,2,2,4),(0.,0.0627614005096921,
0.120088961436388,0.125238462177896),.UNSPECIFIED.);
#1295=B_SPLINE_CURVE_WITH_KNOTS('',3,(#22386,#22387,#22388,#22389,#22390,
#22391,#22392,#22393),.UNSPECIFIED.,.F.,.F.,(4,2,2,4),(0.,0.00526827403022492,
0.0639645578123657,0.128213897069805),.UNSPECIFIED.);
#1296=B_SPLINE_CURVE_WITH_KNOTS('',3,(#22397,#22398,#22399,#22400,#22401,
#22402,#22403,#22404),.UNSPECIFIED.,.F.,.F.,(4,2,2,4),(0.,0.0627613623859368,
0.12008829741618,0.125237359044329),.UNSPECIFIED.);
#1297=B_SPLINE_CURVE_WITH_KNOTS('',3,(#22408,#22409,#22410,#22411,#22412,
#22413,#22414,#22415),.UNSPECIFIED.,.F.,.F.,(4,2,2,4),(0.,0.0052678638691292,
0.0639635307055346,0.128212781223319),.UNSPECIFIED.);
#1298=B_SPLINE_CURVE_WITH_KNOTS('',3,(#22419,#22420,#22421,#22422,#22423,
#22424,#22425,#22426),.UNSPECIFIED.,.F.,.F.,(4,2,2,4),(0.,0.0627613288883452,
0.120087691004123,0.125236352349363),.UNSPECIFIED.);
#1299=B_SPLINE_CURVE_WITH_KNOTS('',3,(#22430,#22431,#22432,#22433,#22434,
#22435,#22436,#22437),.UNSPECIFIED.,.F.,.F.,(4,2,2,4),(0.,0.00526748857527077,
0.0639625889506368,0.128211759700356),.UNSPECIFIED.);
#1300=B_SPLINE_CURVE_WITH_KNOTS('',3,(#22441,#22442,#22443,#22444,#22445,
#22446,#22447,#22448),.UNSPECIFIED.,.F.,.F.,(4,2,2,4),(0.,0.0627622351934734,
0.120057633553872,0.125268887079596),.UNSPECIFIED.);
#1301=B_SPLINE_CURVE_WITH_KNOTS('',3,(#22453,#22454,#22455,#22456,#22457,
#22458),.UNSPECIFIED.,.F.,.F.,(4,2,4),(0.,0.0498589762945784,0.0999595266847454),
 .UNSPECIFIED.);
#1302=B_SPLINE_CURVE_WITH_KNOTS('',3,(#22462,#22463,#22464,#22465,#22466,
#22467,#22468,#22469),.UNSPECIFIED.,.F.,.F.,(4,2,2,4),(0.,0.0627475125621108,
0.120074786005034,0.125235611253279),.UNSPECIFIED.);
#1303=B_SPLINE_CURVE_WITH_KNOTS('',3,(#22473,#22474,#22475,#22476,#22477,
#22478,#22479,#22480),.UNSPECIFIED.,.F.,.F.,(4,2,2,4),(0.,0.00526540507665305,
0.0639607121557458,0.128212582461846),.UNSPECIFIED.);
#1304=B_SPLINE_CURVE_WITH_KNOTS('',3,(#22484,#22485,#22486,#22487,#22488,
#22489,#22490,#22491),.UNSPECIFIED.,.F.,.F.,(4,2,2,4),(0.,0.0627475425879394,
0.120075349322764,0.125236545975591),.UNSPECIFIED.);
#1305=B_SPLINE_CURVE_WITH_KNOTS('',3,(#22495,#22496,#22497,#22498,#22499,
#22500,#22501,#22502),.UNSPECIFIED.,.F.,.F.,(4,2,2,4),(0.,0.00526580973145337,
0.0639617259034633,0.128213683646694),.UNSPECIFIED.);
#1306=B_SPLINE_CURVE_WITH_KNOTS('',3,(#22506,#22507,#22508,#22509,#22510,
#22511,#22512,#22513),.UNSPECIFIED.,.F.,.F.,(4,2,2,4),(0.,0.0627475766076911,
0.120075963575788,0.12523756592846),.UNSPECIFIED.);
#1307=B_SPLINE_CURVE_WITH_KNOTS('',3,(#22517,#22518,#22519,#22520,#22521,
#22522,#22523,#22524),.UNSPECIFIED.,.F.,.F.,(4,2,2,4),(0.,0.00526625387771515,
0.063962836142632,0.128214891577853),.UNSPECIFIED.);
#1308=B_SPLINE_CURVE_WITH_KNOTS('',3,(#22528,#22529,#22530,#22531,#22532,
#22533,#22534,#22535),.UNSPECIFIED.,.F.,.F.,(4,2,2,4),(0.,0.0627476153613634,
0.120076636694826,0.12523868444785),.UNSPECIFIED.);
#1309=B_SPLINE_CURVE_WITH_KNOTS('',3,(#22539,#22540,#22541,#22542,#22543,
#22544,#22545,#22546),.UNSPECIFIED.,.F.,.F.,(4,2,2,4),(0.,0.00526674410433897,
0.063964058787172,0.128216224084347),.UNSPECIFIED.);
#1310=B_SPLINE_CURVE_WITH_KNOTS('',3,(#22550,#22551,#22552,#22553,#22554,
#22555,#22556,#22557),.UNSPECIFIED.,.F.,.F.,(4,2,2,4),(0.,0.0627476597736949,
0.120077378440881,0.125239917954739),.UNSPECIFIED.);
#1311=B_SPLINE_CURVE_WITH_KNOTS('',3,(#22561,#22562,#22563,#22564,#22565,
#22566,#22567,#22568),.UNSPECIFIED.,.F.,.F.,(4,2,2,4),(0.,0.00526728861301724,
0.0639654135345664,0.128217703164965),.UNSPECIFIED.);
#1312=B_SPLINE_CURVE_WITH_KNOTS('',3,(#22572,#22573,#22574,#22575,#22576,
#22577,#22578,#22579),.UNSPECIFIED.,.F.,.F.,(4,2,2,4),(0.,0.0627477110123208,
0.120078200979348,0.125241286926992),.UNSPECIFIED.);
#1313=B_SPLINE_CURVE_WITH_KNOTS('',3,(#22583,#22584,#22585,#22586,#22587,
#22588,#22589,#22590),.UNSPECIFIED.,.F.,.F.,(4,2,2,4),(0.,0.00526789777186566,
0.0639669253649914,0.128219356862823),.UNSPECIFIED.);
#1314=B_SPLINE_CURVE_WITH_KNOTS('',3,(#22596,#22597,#22598,#22599,#22600,
#22601),.UNSPECIFIED.,.F.,.F.,(4,2,4),(0.,0.0322464693148723,0.0645605482559509),
 .UNSPECIFIED.);
#1315=B_SPLINE_CURVE_WITH_KNOTS('',3,(#22605,#22606,#22607,#22608,#22609,
#22610,#22611,#22612),.UNSPECIFIED.,.F.,.F.,(4,2,2,4),(0.,0.0627615225357567,
0.12009094148456,0.125241756269418),.UNSPECIFIED.);
#1316=B_SPLINE_CURVE_WITH_KNOTS('',3,(#22616,#22617,#22618,#22619,#22620,
#22621,#22622,#22623),.UNSPECIFIED.,.F.,.F.,(4,2,2,4),(0.,0.00526949141755586,
0.0639675940491126,0.128217205528332),.UNSPECIFIED.);
#1317=B_SPLINE_CURVE_WITH_KNOTS('',3,(#22627,#22628,#22629,#22630,#22631,
#22632,#22633,#22634),.UNSPECIFIED.,.F.,.F.,(4,2,2,4),(0.,0.0627614683917021,
0.120090086793172,0.125240333549308),.UNSPECIFIED.);
#1318=B_SPLINE_CURVE_WITH_KNOTS('',3,(#22638,#22639,#22640,#22641,#22642,
#22643,#22644,#22645),.UNSPECIFIED.,.F.,.F.,(4,2,2,4),(0.,0.00526896705103507,
0.0639662884118339,0.128215781088997),.UNSPECIFIED.);
#1319=B_SPLINE_CURVE_WITH_KNOTS('',3,(#22649,#22650,#22651,#22652,#22653,
#22654,#22655,#22656),.UNSPECIFIED.,.F.,.F.,(4,2,2,4),(0.,0.0627614215780341,
0.120089317924044,0.125239054744074),.UNSPECIFIED.);
#1320=B_SPLINE_CURVE_WITH_KNOTS('',3,(#22660,#22661,#22662,#22663,#22664,
#22665,#22666,#22667),.UNSPECIFIED.,.F.,.F.,(4,2,2,4),(0.,0.00526849386310405,
0.0639651074163281,0.128214494876759),.UNSPECIFIED.);
#1321=B_SPLINE_CURVE_WITH_KNOTS('',3,(#22671,#22672,#22673,#22674,#22675,
#22676,#22677,#22678),.UNSPECIFIED.,.F.,.F.,(4,2,2,4),(0.,0.0627613808182858,
0.120088621680663,0.125237897640557),.UNSPECIFIED.);
#1322=B_SPLINE_CURVE_WITH_KNOTS('',3,(#22682,#22683,#22684,#22685,#22686,
#22687,#22688,#22689),.UNSPECIFIED.,.F.,.F.,(4,2,2,4),(0.,0.00526806427303071,
0.0639640328250225,0.128213326505552),.UNSPECIFIED.);
#1323=B_SPLINE_CURVE_WITH_KNOTS('',3,(#22693,#22694,#22695,#22696,#22697,
#22698,#22699,#22700),.UNSPECIFIED.,.F.,.F.,(4,2,2,4),(0.,0.0627613451073725,
0.120087987526447,0.125236844511966),.UNSPECIFIED.);
#1324=B_SPLINE_CURVE_WITH_KNOTS('',3,(#22704,#22705,#22706,#22707,#22708,
#22709,#22710,#22711),.UNSPECIFIED.,.F.,.F.,(4,2,2,4),(0.,0.00526767216729547,
0.0639630498969236,0.128212259500237),.UNSPECIFIED.);
#1325=B_SPLINE_CURVE_WITH_KNOTS('',3,(#22715,#22716,#22717,#22718,#22719,
#22720,#22721,#22722),.UNSPECIFIED.,.F.,.F.,(4,2,2,4),(0.,0.0627613136441549,
0.120087406937392,0.125235881024186),.UNSPECIFIED.);
#1326=B_SPLINE_CURVE_WITH_KNOTS('',3,(#22726,#22727,#22728,#22729,#22730,
#22731,#22732,#22733),.UNSPECIFIED.,.F.,.F.,(4,2,2,4),(0.,0.00526731255574918,
0.0639621465613893,0.128211280360621),.UNSPECIFIED.);
#1327=B_SPLINE_CURVE_WITH_KNOTS('',3,(#22737,#22738,#22739,#22740,#22741,
#22742,#22743,#22744),.UNSPECIFIED.,.F.,.F.,(4,2,2,4),(0.,0.0104628362527636,
0.0207308659069718,0.0209057471409188),.UNSPECIFIED.);
#1328=B_SPLINE_CURVE_WITH_KNOTS('',3,(#22748,#22749,#22750,#22751,#22752,
#22753,#22754,#22755,#22756,#22757,#22758,#22759,#22760,#22761,#22762,#22763,
#22764,#22765,#22766,#22767,#22768,#22769,#22770,#22771,#22772,#22773,#22774,
#22775,#22776,#22777,#22778,#22779,#22780,#22781,#22782,#22783,#22784),
 .UNSPECIFIED.,.F.,.F.,(4,3,3,3,3,3,3,3,3,3,3,3,4),(50.7521183952037,50.8495790953441,
50.9470219254028,51.0444588598502,51.1419334813167,51.2394182564582,51.3369688385417,
51.4243296588263,51.5251265267957,51.6212969234942,51.7174260205839,51.8135342633692,
51.827517130704),.UNSPECIFIED.);
#1329=B_SPLINE_CURVE_WITH_KNOTS('',3,(#22787,#22788,#22789,#22790,#22791,
#22792,#22793,#22794,#22795,#22796,#22797,#22798,#22799,#22800,#22801,#22802,
#22803,#22804,#22805,#22806,#22807,#22808,#22809,#22810,#22811,#22812,#22813,
#22814,#22815,#22816,#22817,#22818,#22819,#22820,#22821,#22822,#22823,#22824,
#22825,#22826,#22827,#22828,#22829,#22830,#22831,#22832,#22833,#22834,#22835,
#22836,#22837,#22838,#22839,#22840,#22841,#22842,#22843,#22844,#22845,#22846,
#22847,#22848,#22849,#22850,#22851,#22852,#22853,#22854,#22855,#22856,#22857,
#22858,#22859),.UNSPECIFIED.,.F.,.F.,(4,3,3,3,3,3,3,3,3,3,3,3,3,3,3,3,3,
3,3,3,3,3,3,3,4),(47.6105257416139,47.7077041422575,47.8048611288827,47.9020100199129,
47.999164126441,48.0963691196497,48.1935970979194,48.2908967620636,48.3332993342991,
48.4283008104292,48.5232388584473,48.6181347145911,48.7130095721038,48.8079167672776,
48.9028389899736,48.9978424868404,49.0560729269844,49.1533688574346,49.2506064158459,
49.3477990026261,49.4449599775623,49.5421169168093,49.6392652595687,49.7364384779762,
49.7788465196697),.UNSPECIFIED.);
#1330=B_SPLINE_CURVE_WITH_KNOTS('',3,(#22860,#22861,#22862,#22863,#22864,
#22865,#22866,#22867,#22868,#22869,#22870,#22871,#22872,#22873,#22874,#22875,
#22876,#22877,#22878,#22879,#22880,#22881,#22882,#22883,#22884,#22885,#22886,
#22887,#22888,#22889,#22890,#22891,#22892,#22893,#22894,#22895,#22896,#22897,
#22898,#22899,#22900,#22901,#22902,#22903,#22904,#22905,#22906,#22907,#22908,
#22909,#22910,#22911,#22912,#22913,#22914,#22915,#22916,#22917,#22918,#22919,
#22920,#22921,#22922,#22923,#22924,#22925,#22926,#22927,#22928,#22929,#22930,
#22931,#22932),.UNSPECIFIED.,.F.,.F.,(4,3,3,3,3,3,3,3,3,3,3,3,3,3,3,3,3,
3,3,3,3,3,3,3,4),(47.6105257416139,47.7076886147176,47.8048298475205,47.9019628289092,
47.9991009402533,48.0962899832716,48.1935020701131,48.2907860931928,48.3332993342991,
48.4283243574566,48.523286131773,48.6182058374566,48.7131046117988,48.8080356576868,
48.9029816882567,48.9980087284196,49.0560729269844,49.153353193078,49.2505749096157,
49.3477515476114,49.4448965372306,49.5420376028857,49.6391701728657,49.736327918173,
49.7788465196697),.UNSPECIFIED.);
#1331=B_SPLINE_CURVE_WITH_KNOTS('',3,(#22934,#22935,#22936,#22937,#22938,
#22939,#22940,#22941,#22942,#22943,#22944,#22945,#22946,#22947,#22948,#22949,
#22950,#22951,#22952,#22953,#22954,#22955,#22956,#22957,#22958,#22959,#22960,
#22961,#22962,#22963,#22964,#22965,#22966,#22967,#22968,#22969,#22970,#22971,
#22972,#22973,#22974,#22975,#22976,#22977,#22978,#22979,#22980,#22981,#22982,
#22983,#22984,#22985,#22986,#22987,#22988,#22989,#22990,#22991,#22992,#22993,
#22994,#22995,#22996,#22997,#22998,#22999,#23000,#23001,#23002,#23003,#23004,
#23005,#23006),.UNSPECIFIED.,.F.,.F.,(4,3,3,3,3,3,3,3,3,3,3,3,3,3,3,3,3,
3,3,3,3,3,3,3,4),(44.4689330880241,44.5660877812095,44.6632207148829,44.7603453149378,
44.8574749996526,44.9546556391961,45.0518593530952,45.1491351344189,45.1917066807094,
45.2867442474327,45.3817186612472,45.4766510723439,45.5715625880392,45.6665063398916,
45.7614650533526,45.8565046349539,45.9144802733946,46.011752285669,46.1089656554364,
46.2061338907896,46.3032704588545,46.4004031621129,46.4975274228661,46.5946770168463,
46.6372538660799),.UNSPECIFIED.);
#1332=B_SPLINE_CURVE_WITH_KNOTS('',3,(#23007,#23008,#23009,#23010,#23011,
#23012,#23013,#23014,#23015,#23016,#23017,#23018,#23019,#23020,#23021,#23022,
#23023,#23024,#23025,#23026,#23027,#23028,#23029,#23030,#23031,#23032,#23033,
#23034,#23035,#23036,#23037,#23038,#23039,#23040,#23041,#23042,#23043,#23044,
#23045,#23046,#23047,#23048,#23049,#23050,#23051,#23052,#23053,#23054,#23055,
#23056,#23057,#23058,#23059,#23060,#23061,#23062,#23063,#23064,#23065,#23066,
#23067,#23068,#23069,#23070,#23071,#23072,#23073,#23074,#23075,#23076,#23077,
#23078,#23079),.UNSPECIFIED.,.F.,.F.,(4,3,3,3,3,3,3,3,3,3,3,3,3,3,3,3,3,
3,3,3,3,3,3,3,4),(44.4689330880241,44.5661021364053,44.6632496344749,44.7603889431301,
44.8575334158252,44.954728802457,45.0519472096645,45.149237453745,45.1917066807094,
45.2867222998457,45.3816745984183,45.4765847790615,45.5714740014621,45.6663955218626,
45.7613320441279,45.8563496818008,45.9144802733946,46.0117667696916,46.1089947868675,
46.2061777678908,46.3033291149719,46.4004764935731,46.4976153363918,46.5947792353533,
46.6372538660799),.UNSPECIFIED.);
#1333=B_SPLINE_CURVE_WITH_KNOTS('',3,(#23081,#23082,#23083,#23084,#23085,
#23086,#23087,#23088,#23089,#23090,#23091,#23092,#23093,#23094,#23095,#23096,
#23097,#23098,#23099,#23100,#23101,#23102,#23103,#23104,#23105,#23106,#23107,
#23108,#23109,#23110,#23111,#23112,#23113,#23114,#23115,#23116,#23117,#23118,
#23119,#23120,#23121,#23122,#23123,#23124,#23125,#23126,#23127,#23128,#23129,
#23130,#23131,#23132,#23133,#23134,#23135,#23136,#23137,#23138,#23139,#23140,
#23141,#23142,#23143,#23144,#23145,#23146,#23147,#23148,#23149,#23150,#23151,
#23152,#23153),.UNSPECIFIED.,.F.,.F.,(4,3,3,3,3,3,3,3,3,3,3,3,3,3,3,3,3,
3,3,3,3,3,3,3,4),(41.3273404344343,41.4245008426539,41.5216395746521,41.6187700304753,
41.7159056026232,41.8130921134644,41.9103016773613,42.0075832170803,42.0501140271196,
42.1451428193501,42.2401083915334,42.3350319148704,42.4299345176583,42.5248693813708,
42.6198192228509,42.7148500314578,42.7728876198048,42.8701653988873,42.9673846003622,
43.0645587064248,43.1617011583864,43.2588397041862,43.3559697703269,43.4531250593715,
43.4956612124901),.UNSPECIFIED.);
#1334=B_SPLINE_CURVE_WITH_KNOTS('',3,(#23154,#23155,#23156,#23157,#23158,
#23159,#23160,#23161,#23162,#23163,#23164,#23165,#23166,#23167,#23168,#23169,
#23170,#23171,#23172,#23173,#23174,#23175,#23176,#23177,#23178,#23179,#23180,
#23181,#23182,#23183,#23184,#23185,#23186,#23187,#23188,#23189,#23190,#23191,
#23192,#23193,#23194,#23195,#23196,#23197,#23198,#23199,#23200,#23201,#23202,
#23203,#23204,#23205,#23206,#23207,#23208,#23209,#23210,#23211,#23212,#23213,
#23214,#23215,#23216,#23217,#23218,#23219,#23220,#23221,#23222,#23223,#23224,
#23225,#23226),.UNSPECIFIED.,.F.,.F.,(4,3,3,3,3,3,3,3,3,3,3,3,3,3,3,3,3,
3,3,3,3,3,3,3,4),(41.3273404344343,41.4244875449837,41.5216127854883,41.6187296160768,
41.7158514891715,41.8130243381864,41.9102202895791,42.0074884295393,42.0501140271195,
42.1451633170348,42.2401495439751,42.3350938299693,42.4300172542117,42.5249728814293,
42.6199434485318,42.7149947512481,42.7728876198048,42.8701519796663,42.9673576112281,
43.0645180568829,43.1616468179474,43.2587717692632,43.3558883274192,43.4530303652185,
43.4956612124901),.UNSPECIFIED.);
#1335=B_SPLINE_CURVE_WITH_KNOTS('',3,(#23228,#23229,#23230,#23231,#23232,
#23233,#23234,#23235,#23236,#23237,#23238,#23239,#23240,#23241,#23242,#23243,
#23244,#23245,#23246,#23247,#23248,#23249,#23250,#23251,#23252,#23253,#23254,
#23255,#23256,#23257,#23258,#23259,#23260,#23261,#23262,#23263,#23264,#23265,
#23266,#23267,#23268,#23269,#23270,#23271,#23272,#23273,#23274,#23275,#23276,
#23277,#23278,#23279,#23280,#23281,#23282,#23283,#23284,#23285,#23286,#23287,
#23288,#23289,#23290,#23291,#23292,#23293,#23294,#23295,#23296,#23297,#23298,
#23299,#23300),.UNSPECIFIED.,.F.,.F.,(4,3,3,3,3,3,3,3,3,3,3,3,3,3,3,3,3,
3,3,3,3,3,3,3,4),(38.1857477808445,38.2828878496606,38.3800059457443,38.4771155609571,
38.5742301793694,38.6713957929425,38.7685845346598,38.8658455770237,38.9085213735298,
39.0035816400817,39.0985789281084,39.1935343331749,39.2884689080497,39.383435654736,
39.478417320826,39.5734795981558,39.631294966215,39.7285522183372,39.8257506628246,
39.9229038738615,40.0200253844543,40.1171431366437,40.2142525415632,40.3113875621596,
40.3540685589003),.UNSPECIFIED.);
#1336=B_SPLINE_CURVE_WITH_KNOTS('',3,(#23301,#23302,#23303,#23304,#23305,
#23306,#23307,#23308,#23309,#23310,#23311,#23312,#23313,#23314,#23315,#23316,
#23317,#23318,#23319,#23320,#23321,#23322,#23323,#23324,#23325,#23326,#23327,
#23328,#23329,#23330,#23331,#23332,#23333,#23334,#23335,#23336,#23337,#23338,
#23339,#23340,#23341,#23342,#23343,#23344,#23345,#23346,#23347,#23348,#23349,
#23350,#23351,#23352,#23353,#23354,#23355,#23356,#23357,#23358,#23359,#23360,
#23361,#23362,#23363,#23364,#23365,#23366,#23367,#23368,#23369,#23370,#23371,
#23372,#23373),.UNSPECIFIED.,.F.,.F.,(4,3,3,3,3,3,3,3,3,3,3,3,3,3,3,3,3,
3,3,3,3,3,3,3,4),(38.1857477808445,38.2829001906186,38.3800308075986,38.4771530679947,
38.5742804003744,38.6714586939732,38.7686600703952,38.8659335507706,38.9085213735298,
39.0035624604914,39.0985404215215,39.1934763983655,39.2883914899063,39.3833388076511,
39.4783010804979,39.5733441817229,39.631294966215,39.7285646742001,39.8257757138043,
39.9229416034566,40.0200758205865,40.1172061894662,40.214328130694,40.3114754492342,
40.3540685589003),.UNSPECIFIED.);
#1337=B_SPLINE_CURVE_WITH_KNOTS('',3,(#23375,#23376,#23377,#23378,#23379,
#23380,#23381,#23382,#23383,#23384,#23385,#23386,#23387,#23388,#23389,#23390,
#23391,#23392,#23393,#23394,#23395,#23396,#23397,#23398,#23399,#23400,#23401,
#23402,#23403,#23404,#23405,#23406,#23407,#23408,#23409,#23410,#23411,#23412,
#23413,#23414,#23415,#23416,#23417,#23418,#23419,#23420,#23421,#23422,#23423,
#23424,#23425,#23426,#23427,#23428,#23429,#23430,#23431,#23432,#23433,#23434,
#23435,#23436,#23437,#23438,#23439,#23440,#23441,#23442,#23443,#23444,#23445,
#23446,#23447),.UNSPECIFIED.,.F.,.F.,(4,3,3,3,3,3,3,3,3,3,3,3,3,3,3,3,3,
3,3,3,3,3,3,3,4),(35.0441551272547,35.1413001185802,35.2384232089616,35.3355378680837,
35.4326575578995,35.5298282294624,35.6270220111843,35.724288015248,35.76692871994,
35.8619813038615,35.956970850126,36.0519184728304,36.1468452432485,36.2418042072995,
36.3367781051034,36.4318327012268,36.4897023126252,36.5869645335255,36.6841680022149,
36.7813262706603,36.8784528497216,36.9755756344637,37.0726900398495,37.1698299658108,
37.2124759053105),.UNSPECIFIED.);
#1338=B_SPLINE_CURVE_WITH_KNOTS('',3,(#23448,#23449,#23450,#23451,#23452,
#23453,#23454,#23455,#23456,#23457,#23458,#23459,#23460,#23461,#23462,#23463,
#23464,#23465,#23466,#23467,#23468,#23469,#23470,#23471,#23472,#23473,#23474,
#23475,#23476,#23477,#23478,#23479,#23480,#23481,#23482,#23483,#23484,#23485,
#23486,#23487,#23488,#23489,#23490,#23491,#23492,#23493,#23494,#23495,#23496,
#23497,#23498,#23499,#23500,#23501,#23502,#23503,#23504,#23505,#23506,#23507,
#23508,#23509,#23510,#23511,#23512,#23513,#23514,#23515,#23516,#23517,#23518,
#23519,#23520),.UNSPECIFIED.,.F.,.F.,(4,3,3,3,3,3,3,3,3,3,3,3,3,3,3,3,3,
3,3,3,3,3,3,3,4),(35.0441551272547,35.1412886454812,35.2384000954,35.3355029983402,
35.4326108677603,35.5297697499161,35.6269517839495,35.7242062225055,35.76692871994,
35.8619992819673,35.9570069448942,36.0519727793798,36.1469178133221,36.2418949897621,
36.336887066271,36.4319596371093,36.4897023126252,36.5869529516101,36.6841447094667,
36.7812911898994,36.8784059553419,36.9755170103548,37.0726197608562,37.1697482536537,
37.2124759053105),.UNSPECIFIED.);
#1339=B_SPLINE_CURVE_WITH_KNOTS('',3,(#23522,#23523,#23524,#23525,#23526,
#23527,#23528,#23529,#23530,#23531,#23532,#23533,#23534,#23535,#23536,#23537,
#23538,#23539,#23540,#23541,#23542,#23543,#23544,#23545,#23546,#23547,#23548,
#23549,#23550,#23551,#23552,#23553,#23554,#23555,#23556,#23557,#23558,#23559,
#23560,#23561,#23562,#23563,#23564,#23565,#23566,#23567,#23568,#23569,#23570,
#23571,#23572,#23573,#23574,#23575,#23576,#23577,#23578,#23579,#23580,#23581,
#23582,#23583,#23584,#23585,#23586,#23587,#23588,#23589,#23590,#23591,#23592,
#23593,#23594),.UNSPECIFIED.,.F.,.F.,(4,3,3,3,3,3,3,3,3,3,3,3,3,3,3,3,3,
3,3,3,3,3,3,3,4),(31.9025624736649,31.9996898883771,32.096795145671,32.193891794287,
32.2909933750212,32.3881459845633,32.4853217678791,32.5825700521498,32.6253360663502,
32.7204163008207,32.8154337110007,32.9104093440756,33.0053642045037,33.1003511798146,
33.1953530369193,33.2904352782913,33.3481096590354,33.4453541351378,33.5425396619171,
33.6396798705364,33.7367883508018,33.8338931655412,33.9309897156823,34.0281121261795,
34.0708832517207),.UNSPECIFIED.);
#1340=B_SPLINE_CURVE_WITH_KNOTS('',3,(#23595,#23596,#23597,#23598,#23599,
#23600,#23601,#23602,#23603,#23604,#23605,#23606,#23607,#23608,#23609,#23610,
#23611,#23612,#23613,#23614,#23615,#23616,#23617,#23618,#23619,#23620,#23621,
#23622,#23623,#23624,#23625,#23626,#23627,#23628,#23629,#23630,#23631,#23632,
#23633,#23634,#23635,#23636,#23637,#23638,#23639,#23640,#23641,#23642,#23643,
#23644,#23645,#23646,#23647,#23648,#23649,#23650,#23651,#23652,#23653,#23654,
#23655,#23656,#23657,#23658,#23659,#23660,#23661,#23662,#23663,#23664,#23665,
#23666,#23667),.UNSPECIFIED.,.F.,.F.,(4,3,3,3,3,3,3,3,3,3,3,3,3,3,3,3,3,
3,3,3,3,3,3,3,4),(31.9025624736649,31.9997005722075,32.0968166692765,32.1939242656021,
32.291036854099,32.3882004430768,32.4853871673618,32.5826462235772,32.6253360663502,
32.7203994206752,32.8153998202737,32.9103583532498,33.0052960649213,33.1002659396212,
33.1952507279387,33.2903160924587,33.3481096590354,33.445364922192,33.5425613555767,
33.6397125422578,33.7368320240988,33.8339477619433,33.9310551653709,34.0281882225514,
34.0708832517207),.UNSPECIFIED.);
#1341=B_SPLINE_CURVE_WITH_KNOTS('',3,(#23669,#23670,#23671,#23672,#23673,
#23674,#23675,#23676,#23677,#23678,#23679,#23680,#23681,#23682,#23683,#23684,
#23685,#23686,#23687,#23688,#23689,#23690,#23691,#23692,#23693,#23694,#23695,
#23696,#23697,#23698,#23699,#23700,#23701,#23702,#23703,#23704,#23705,#23706,
#23707,#23708,#23709,#23710,#23711,#23712,#23713,#23714,#23715,#23716,#23717,
#23718,#23719,#23720,#23721,#23722,#23723,#23724,#23725,#23726,#23727,#23728,
#23729,#23730,#23731,#23732,#23733,#23734,#23735,#23736,#23737,#23738,#23739,
#23740,#23741),.UNSPECIFIED.,.F.,.F.,(4,3,3,3,3,3,3,3,3,3,3,3,3,3,3,3,3,
3,3,3,3,3,3,3,4),(28.7609698200751,28.8581015035,28.9552110918357,29.0523121146564,
29.1494180936432,29.246575090229,29.3437552452973,29.4410078339139,29.4837434127604,
29.5788168740845,29.6738274587129,29.7687962302759,29.8637442096533,29.9587243232585,
30.053719331466,30.148794801035,30.2065170054456,30.3037657918968,30.4009556766901,
30.498100271789,30.5952131478604,30.6923223269791,30.7894232135769,30.886549877952,
30.9292905981309),.UNSPECIFIED.);
#1342=B_SPLINE_CURVE_WITH_KNOTS('',3,(#23742,#23743,#23744,#23745,#23746,
#23747,#23748,#23749,#23750,#23751,#23752,#23753,#23754,#23755,#23756,#23757,
#23758,#23759,#23760,#23761,#23762,#23763,#23764,#23765,#23766,#23767,#23768,
#23769,#23770,#23771,#23772,#23773,#23774,#23775,#23776,#23777,#23778,#23779,
#23780,#23781,#23782,#23783,#23784,#23785,#23786,#23787,#23788,#23789,#23790,
#23791,#23792,#23793,#23794,#23795,#23796,#23797,#23798,#23799,#23800,#23801,
#23802,#23803,#23804,#23805,#23806,#23807,#23808,#23809,#23810,#23811,#23812,
#23813,#23814),.UNSPECIFIED.,.F.,.F.,(4,3,3,3,3,3,3,3,3,3,3,3,3,3,3,3,3,
3,3,3,3,3,3,3,4),(28.7609698200751,28.8580915391914,28.95519101767,29.0522818297916,
29.1493775418228,29.2465242973753,29.3436942469329,29.4409367871068,29.4837434127604,
29.5788327484787,29.6738593304695,29.7688441837639,29.863808290698,29.9588044864641,
30.0538155467294,30.1489068874975,30.2065170054456,30.3037557295149,30.4009354408839,
30.498069796299,30.5951724110685,30.6922714024132,30.7893621664804,30.8864789011626,
30.9292905981309),.UNSPECIFIED.);
#1343=B_SPLINE_CURVE_WITH_KNOTS('',3,(#23816,#23817,#23818,#23819,#23820,
#23821,#23822,#23823,#23824,#23825,#23826,#23827,#23828,#23829,#23830,#23831,
#23832,#23833,#23834,#23835,#23836,#23837,#23838,#23839,#23840,#23841,#23842,
#23843,#23844,#23845,#23846,#23847,#23848,#23849,#23850,#23851,#23852,#23853,
#23854,#23855,#23856,#23857,#23858,#23859,#23860,#23861,#23862,#23863,#23864,
#23865,#23866,#23867,#23868,#23869,#23870,#23871,#23872,#23873,#23874,#23875,
#23876,#23877,#23878,#23879,#23880,#23881,#23882,#23883,#23884,#23885,#23886,
#23887,#23888),.UNSPECIFIED.,.F.,.F.,(4,3,3,3,3,3,3,3,3,3,3,3,3,3,3,3,3,
3,3,3,3,3,3,3,4),(25.6193771664853,25.716493563024,25.813587641087,25.9106729987879,
26.0077632261613,26.1049045105381,26.2020690076394,26.2993061788448,26.3421507591706,
26.4372486713073,26.5322838963633,26.6272774384332,26.7222502589474,26.8172551436848,
26.9122748765366,27.0073747919292,27.0649243518559,27.1621576996185,27.2593319756947,
27.356460860703,27.4535579937485,27.5506515429054,27.6477368997384,27.7448483303182,
27.7876979445411),.UNSPECIFIED.);
#1344=B_SPLINE_CURVE_WITH_KNOTS('',3,(#23889,#23890,#23891,#23892,#23893,
#23894,#23895,#23896,#23897,#23898,#23899,#23900,#23901,#23902,#23903,#23904,
#23905,#23906,#23907,#23908,#23909,#23910,#23911,#23912,#23913,#23914,#23915,
#23916,#23917,#23918,#23919,#23920,#23921,#23922,#23923,#23924,#23925,#23926,
#23927,#23928,#23929,#23930,#23931,#23932,#23933,#23934,#23935,#23936,#23937,
#23938,#23939,#23940,#23941,#23942,#23943,#23944,#23945,#23946,#23947,#23948,
#23949,#23950,#23951,#23952,#23953,#23954,#23955,#23956,#23957,#23958,#23959,
#23960,#23961),.UNSPECIFIED.,.F.,.F.,(4,3,3,3,3,3,3,3,3,3,3,3,3,3,3,3,3,
3,3,3,3,3,3,3,4),(25.6193771664853,25.7165028699044,25.8136063909083,25.9107012859153,
26.0078011033783,26.1049519540998,26.2021259846947,26.2993725432181,26.3421507591706,
26.4372337202794,26.5322538782203,26.6272322735482,26.7221899041007,26.8171796417382,
26.9121842559982,27.0072692234594,27.0649243518558,27.1621670998174,27.2593508793865,
27.3564893294171,27.4535960473819,27.5506991124494,27.6477939241238,27.7449146292726,
27.7876979445411),.UNSPECIFIED.);
#1345=B_SPLINE_CURVE_WITH_KNOTS('',3,(#23963,#23964,#23965,#23966,#23967,
#23968,#23969,#23970,#23971,#23972,#23973,#23974,#23975,#23976,#23977,#23978,
#23979,#23980,#23981,#23982,#23983,#23984,#23985,#23986,#23987,#23988,#23989,
#23990,#23991,#23992,#23993,#23994,#23995,#23996,#23997,#23998,#23999,#24000,
#24001,#24002,#24003,#24004,#24005,#24006,#24007,#24008,#24009,#24010,#24011,
#24012,#24013,#24014,#24015,#24016,#24017,#24018,#24019,#24020,#24021,#24022,
#24023,#24024,#24025,#24026,#24027,#24028,#24029,#24030,#24031,#24032,#24033,
#24034,#24035),.UNSPECIFIED.,.F.,.F.,(4,3,3,3,3,3,3,3,3,3,3,3,3,3,3,3,3,
3,3,3,3,3,3,3,4),(22.4777845128955,22.5749046335756,22.6720024902499,22.7690916643597,
22.866185729313,22.9633308418649,23.060499154063,23.1577400819812,23.2005581055808,
23.2956500094129,23.3906791794585,23.4856666344857,23.5806333505766,23.6756321481368,
23.7706458052989,23.8657397136487,23.9233316982661,24.0205688078678,24.11774688703,
24.2148795996717,24.3119805682513,24.4090779252588,24.5061670654776,24.6032822072728,
24.6461052909513),.UNSPECIFIED.);
#1346=B_SPLINE_CURVE_WITH_KNOTS('',3,(#24036,#24037,#24038,#24039,#24040,
#24041,#24042,#24043,#24044,#24045,#24046,#24047,#24048,#24049,#24050,#24051,
#24052,#24053,#24054,#24055,#24056,#24057,#24058,#24059,#24060,#24061,#24062,
#24063,#24064,#24065,#24066,#24067,#24068,#24069,#24070,#24071,#24072,#24073,
#24074,#24075,#24076,#24077,#24078,#24079,#24080,#24081,#24082,#24083,#24084,
#24085,#24086,#24087,#24088,#24089,#24090,#24091,#24092,#24093,#24094,#24095,
#24096,#24097,#24098,#24099,#24100,#24101,#24102,#24103,#24104,#24105,#24106,
#24107,#24108),.UNSPECIFIED.,.F.,.F.,(4,3,3,3,3,3,3,3,3,3,3,3,3,3,3,3,3,
3,3,3,3,3,3,3,4),(22.4777845128955,22.5748959286778,22.671984953073,22.7690652064669,
22.8661503011054,22.9632864651105,23.0604458591832,23.1576780052064,23.2005581055808,
23.2956641108984,23.390707492164,23.4857092336619,23.5806902770408,23.6757033613676,
23.7707312782682,23.865839285105,23.9233316982661,24.0205600140509,24.1177292031745,
24.2148529685625,24.311944971558,24.4090334278485,24.5061137246012,24.6032201917074,
24.6461052909513),.UNSPECIFIED.);
#1347=B_SPLINE_CURVE_WITH_KNOTS('',3,(#24110,#24111,#24112,#24113,#24114,
#24115,#24116,#24117,#24118,#24119,#24120,#24121,#24122,#24123,#24124,#24125,
#24126,#24127,#24128,#24129,#24130,#24131,#24132,#24133,#24134,#24135,#24136,
#24137,#24138,#24139,#24140,#24141,#24142,#24143,#24144,#24145,#24146,#24147,
#24148,#24149,#24150,#24151,#24152,#24153,#24154,#24155,#24156,#24157,#24158,
#24159,#24160,#24161,#24162,#24163,#24164,#24165,#24166,#24167,#24168,#24169,
#24170,#24171,#24172,#24173,#24174,#24175,#24176,#24177,#24178,#24179,#24180,
#24181,#24182),.UNSPECIFIED.,.F.,.F.,(4,3,3,3,3,3,3,3,3,3,3,3,3,3,3,3,3,
3,3,3,3,3,3,3,4),(19.3361918593058,19.4332986081893,19.5303828972939,19.6274583678477,
19.7245386528814,19.8216700186272,19.9188246305281,20.0160520670602,20.058965451991,
20.1540791046628,20.2491301929626,20.3441396824075,20.4391284959064,20.5341493283117,
20.6291849785355,20.724300631046,20.7817390446763,20.8789626446681,20.9761270666951,
21.0732460345572,21.1703332304066,21.2674169145724,21.3644924699983,21.4615942863967,
21.5045126373615),.UNSPECIFIED.);
#1348=B_SPLINE_CURVE_WITH_KNOTS('',3,(#24183,#24184,#24185,#24186,#24187,
#24188,#24189,#24190,#24191,#24192,#24193,#24194,#24195,#24196,#24197,#24198,
#24199,#24200,#24201,#24202,#24203,#24204,#24205,#24206,#24207,#24208,#24209,
#24210,#24211,#24212,#24213,#24214,#24215,#24216,#24217,#24218,#24219,#24220,
#24221,#24222,#24223,#24224,#24225,#24226,#24227,#24228,#24229,#24230,#24231,
#24232,#24233,#24234,#24235,#24236,#24237,#24238,#24239,#24240,#24241,#24242,
#24243,#24244,#24245,#24246,#24247,#24248,#24249,#24250,#24251,#24252,#24253,
#24254,#24255),.UNSPECIFIED.,.F.,.F.,(4,3,3,3,3,3,3,3,3,3,3,3,3,3,3,3,3,
3,3,3,3,3,3,3,4),(19.3361918593058,19.4333067607529,19.5303993218462,19.6274831473878,
19.7245718340825,19.8217115815184,19.9188745469029,20.016110209788,20.058965451991,
20.1540657863833,20.2491034525452,20.3440994486475,20.4390747302055,20.5340820690261,
20.6291042513177,20.7242065884507,20.7817390446763,20.8789708820714,20.9761436312549,
21.0732709795444,21.1703665727236,21.267458593156,21.3645424310974,21.461652371774,
21.5045126373615),.UNSPECIFIED.);
#1349=B_SPLINE_CURVE_WITH_KNOTS('',3,(#24257,#24258,#24259,#24260,#24261,
#24262,#24263,#24264,#24265,#24266,#24267,#24268,#24269,#24270,#24271,#24272,
#24273,#24274,#24275,#24276,#24277,#24278,#24279,#24280,#24281,#24282,#24283,
#24284,#24285,#24286,#24287,#24288,#24289,#24290,#24291,#24292,#24293,#24294,
#24295,#24296,#24297,#24298,#24299,#24300,#24301,#24302,#24303,#24304,#24305,
#24306,#24307,#24308,#24309,#24310,#24311,#24312,#24313,#24314,#24315,#24316,
#24317,#24318,#24319,#24320,#24321,#24322,#24323,#24324,#24325,#24326,#24327,
#24328,#24329),.UNSPECIFIED.,.F.,.F.,(4,3,3,3,3,3,3,3,3,3,3,3,3,3,3,3,3,
3,3,3,3,3,3,3,4),(16.194599205716,16.2917092212331,16.3887968248508,16.4858756432112,
16.582959294799,16.6800940191828,16.7772519784781,16.8744827115582,16.9173727984012,
17.0124810914989,17.1075267783859,17.2025308377369,17.2975142055994,17.3925296078208,
17.487559838209,17.5826701323273,17.6401463910865,17.7373732920307,17.8345410508988,
17.9316633768824,18.028753937571,18.1258409620435,18.2229198362103,18.3200249079094,
18.3629199837717),.UNSPECIFIED.);
#1350=B_SPLINE_CURVE_WITH_KNOTS('',3,(#24330,#24331,#24332,#24333,#24334,
#24335,#24336,#24337,#24338,#24339,#24340,#24341,#24342,#24343,#24344,#24345,
#24346,#24347,#24348,#24349,#24350,#24351,#24352,#24353,#24354,#24355,#24356,
#24357,#24358,#24359,#24360,#24361,#24362,#24363,#24364,#24365,#24366,#24367,
#24368,#24369,#24370,#24371,#24372,#24373,#24374,#24375,#24376,#24377,#24378,
#24379,#24380,#24381,#24382,#24383,#24384,#24385,#24386,#24387,#24388,#24389,
#24390,#24391,#24392,#24393,#24394,#24395,#24396,#24397,#24398,#24399,#24400,
#24401,#24402),.UNSPECIFIED.,.F.,.F.,(4,3,3,3,3,3,3,3,3,3,3,3,3,3,3,3,3,
3,3,3,3,3,3,3,4),(16.194599205716,16.2917015764267,16.3887814231217,16.4858524065585,
16.582928179243,16.680055043057,16.7772051679657,16.8744281854468,16.9173727984012,
17.0124936863374,17.1075520664769,17.2025688865374,17.2975650516549,17.3925932147811,
17.4876361817024,17.5827590678518,17.6401463910865,17.7373655661754,17.8345255153633,
17.9316399820084,18.0287226677607,18.125801874859,18.2228729821873,18.3199704356026,
18.3629199837717),.UNSPECIFIED.);
#1351=B_SPLINE_CURVE_WITH_KNOTS('',3,(#24404,#24405,#24406,#24407,#24408,
#24409,#24410,#24411,#24412,#24413,#24414,#24415,#24416,#24417,#24418,#24419,
#24420,#24421,#24422,#24423,#24424,#24425,#24426,#24427,#24428,#24429,#24430,
#24431,#24432,#24433,#24434,#24435,#24436,#24437,#24438,#24439,#24440,#24441,
#24442,#24443,#24444,#24445,#24446,#24447,#24448,#24449,#24450,#24451,#24452,
#24453,#24454,#24455,#24456,#24457,#24458,#24459,#24460,#24461,#24462,#24463,
#24464,#24465,#24466,#24467,#24468,#24469,#24470,#24471,#24472,#24473,#24474,
#24475,#24476),.UNSPECIFIED.,.F.,.F.,(4,3,3,3,3,3,3,3,3,3,3,3,3,3,3,3,3,
3,3,3,3,3,3,3,4),(13.0530065521262,13.1501048107483,13.2471804849447,13.3442472537944,
13.4413187880749,13.5384414230539,13.635587333016,13.7328061991352,13.7757801448114,
13.8709078864207,13.9659731739255,14.0609969381436,14.1560000673363,14.2510351747027,
14.3460850725229,14.4412148107737,14.4985537374967,14.5957687557829,14.692924503326,
14.7900347418324,14.8871131912435,14.9841881931923,15.0812551226574,15.1783484782532,
15.2213273301819),.UNSPECIFIED.);
#1352=B_SPLINE_CURVE_WITH_KNOTS('',3,(#24477,#24478,#24479,#24480,#24481,
#24482,#24483,#24484,#24485,#24486,#24487,#24488,#24489,#24490,#24491,#24492,
#24493,#24494,#24495,#24496,#24497,#24498,#24499,#24500,#24501,#24502,#24503,
#24504,#24505,#24506,#24507,#24508,#24509,#24510,#24511,#24512,#24513,#24514,
#24515,#24516,#24517,#24518,#24519,#24520,#24521,#24522,#24523,#24524,#24525,
#24526,#24527,#24528,#24529,#24530,#24531,#24532,#24533,#24534,#24535,#24536,
#24537,#24538,#24539,#24540,#24541,#24542,#24543,#24544,#24545,#24546,#24547,
#24548,#24549),.UNSPECIFIED.,.F.,.F.,(4,3,3,3,3,3,3,3,3,3,3,3,3,3,3,3,3,
3,3,3,3,3,3,3,4),(13.0530065521262,13.1501119879219,13.2471949446812,13.3442690694918,
13.4413480012277,13.538478016824,13.6356312830718,13.7328573943529,13.7757801448114,
13.8708959610436,13.9659492298102,14.06096091131,14.155951923142,14.2509749476356,
14.3460127857609,14.4411306013495,14.4985537374967,14.5957760104763,14.692939091094,
14.790056709018,14.8871425522508,14.9842248936878,15.081299115065,15.178399622931,
15.2213273301819),.UNSPECIFIED.);
#1353=B_SPLINE_CURVE_WITH_KNOTS('',3,(#24552,#24553,#24554,#24555,#24556,
#24557,#24558,#24559,#24560,#24561,#24562,#24563,#24564,#24565,#24566,#24567,
#24568,#24569,#24570,#24571,#24572,#24573,#24574,#24575,#24576,#24577,#24578,
#24579,#24580,#24581,#24582,#24583,#24584,#24585,#24586,#24587,#24588,#24589,
#24590,#24591,#24592,#24593,#24594,#24595,#24596,#24597,#24598,#24599,#24600,
#24601,#24602,#24603,#24604,#24605,#24606,#24607,#24608,#24609),
 .UNSPECIFIED.,.F.,.F.,(4,3,3,3,3,3,3,3,3,3,3,3,3,3,3,3,3,3,3,4),(10.3759343473738,
10.4776920151116,10.5797615894555,10.6818311637994,10.7772132685231,10.8725374348761,
10.9678238901407,11.0630928222215,11.1583925295894,11.2537087060563,11.349094925203,
11.3807829201958,11.4781327140782,11.5754282226452,11.672682517207,11.7744455570533,
11.8716690282138,11.9688871995782,12.0661275540112,12.0797346765921),
 .UNSPECIFIED.);
#1354=B_SPLINE_CURVE_WITH_KNOTS('',3,(#24612,#24613,#24614,#24615,#24616,
#24617),.UNSPECIFIED.,.F.,.F.,(4,2,4),(-0.150154721215487,-0.0750760525081923,
0.),.UNSPECIFIED.);
#1355=B_SPLINE_CURVE_WITH_KNOTS('',3,(#24635,#24636,#24637,#24638),
 .UNSPECIFIED.,.F.,.F.,(4,4),(0.,0.349249092707648),.UNSPECIFIED.);
#1356=B_SPLINE_CURVE_WITH_KNOTS('',3,(#24665,#24666,#24667,#24668,#24669,
#24670,#24671,#24672,#24673,#24674,#24675,#24676,#24677,#24678,#24679,#24680,
#24681,#24682,#24683,#24684,#24685,#24686,#24687,#24688,#24689,#24690,#24691,
#24692,#24693,#24694,#24695,#24696,#24697,#24698,#24699,#24700,#24701,#24702,
#24703,#24704,#24705,#24706,#24707,#24708,#24709,#24710,#24711,#24712,#24713),
 .UNSPECIFIED.,.F.,.F.,(4,3,3,3,3,3,3,3,3,3,3,3,3,3,3,3,4),(0.,0.0365327394137222,
0.0731538029954259,0.109091394005677,0.13300952667614,0.146488998493649,
0.154604853715662,0.189906058994596,0.204763924687531,0.24043732279748,
0.276031768568226,0.295512148258635,0.303306009056309,0.338045252946507,
0.372662891911848,0.40666751045333,0.414264078313279),.UNSPECIFIED.);
#1357=B_SPLINE_CURVE_WITH_KNOTS('',3,(#24714,#24715,#24716,#24717,#24718),
 .UNSPECIFIED.,.F.,.F.,(4,1,4),(39.5699522859152,40.0185665844411,40.2123859659494),
 .UNSPECIFIED.);
#1358=B_SPLINE_CURVE_WITH_KNOTS('',3,(#24743,#24744,#24745,#24746,#24747,
#24748),.UNSPECIFIED.,.F.,.F.,(4,1,1,4),(33.2867669787356,33.7353812772616,
34.4581548699468,34.9067691684727),.UNSPECIFIED.);
#1359=B_SPLINE_CURVE_WITH_KNOTS('',3,(#24773,#24774,#24775,#24776,#24777,
#24778),.UNSPECIFIED.,.F.,.F.,(4,1,1,4),(27.003581671556,27.452195970082,
28.1749695627672,28.6235838612931),.UNSPECIFIED.);
#1360=B_SPLINE_CURVE_WITH_KNOTS('',3,(#24803,#24804,#24805,#24806,#24807,
#24808),.UNSPECIFIED.,.F.,.F.,(4,1,1,4),(20.7203963643765,21.1690106629024,
21.8917842555876,22.3403985541136),.UNSPECIFIED.);
#1361=B_SPLINE_CURVE_WITH_KNOTS('',3,(#24833,#24834,#24835,#24836,#24837,
#24838),.UNSPECIFIED.,.F.,.F.,(4,1,1,4),(14.4372110571969,14.8858253557228,
15.608598948408,16.057213246934),.UNSPECIFIED.);
#1362=B_SPLINE_CURVE_WITH_KNOTS('',3,(#24863,#24864,#24865,#24866,#24867,
#24868),.UNSPECIFIED.,.F.,.F.,(4,1,1,4),(8.15402575001729,8.60264004854321,
9.32541364122847,9.77402793975438),.UNSPECIFIED.);
#1363=B_SPLINE_CURVE_WITH_KNOTS('',3,(#24893,#24894,#24895,#24896,#24897,
#24898,#24899,#24900,#24901,#24902,#24903,#24904,#24905,#24906,#24907,#24908,
#24909,#24910,#24911,#24912,#24913,#24914,#24915,#24916,#24917,#24918,#24919,
#24920,#24921,#24922,#24923,#24924,#24925,#24926,#24927,#24928,#24929,#24930,
#24931,#24932,#24933,#24934,#24935,#24936,#24937,#24938,#24939,#24940,#24941,
#24942,#24943,#24944,#24945,#24946,#24947,#24948,#24949,#24950),
 .UNSPECIFIED.,.F.,.F.,(4,3,3,3,3,3,3,3,3,3,3,3,3,3,3,3,3,3,3,4),(1.87084044283771,
1.96325029725783,2.05566622969097,2.14812754057612,2.24061018839636,2.33315480194847,
2.36709841394138,2.45784756460922,2.54854382431794,2.63920461494343,2.72984732525151,
2.82051706645472,2.91119807753201,3.00194817584722,3.06605017033776,3.1596597536536,
3.2532033890349,3.34670011823176,3.44015197236434,3.49084263257479),
 .UNSPECIFIED.);
#1364=B_SPLINE_CURVE_WITH_KNOTS('',3,(#24976,#24977,#24978,#24979,#24980,
#24981),.UNSPECIFIED.,.F.,.F.,(4,1,1,4),(36.4283596323254,36.8769739308513,
37.5997475235366,38.0483618220625),.UNSPECIFIED.);
#1365=B_SPLINE_CURVE_WITH_KNOTS('',3,(#25006,#25007,#25008,#25009,#25010,
#25011),.UNSPECIFIED.,.F.,.F.,(4,1,1,4),(30.1451743251458,30.5937886236718,
31.316562216357,31.7651765148829),.UNSPECIFIED.);
#1366=B_SPLINE_CURVE_WITH_KNOTS('',3,(#25036,#25037,#25038,#25039,#25040,
#25041),.UNSPECIFIED.,.F.,.F.,(4,1,1,4),(23.8619890179663,24.3106033164922,
25.0333769091774,25.4819912077033),.UNSPECIFIED.);
#1367=B_SPLINE_CURVE_WITH_KNOTS('',3,(#25066,#25067,#25068,#25069,#25070,
#25071),.UNSPECIFIED.,.F.,.F.,(4,1,1,4),(17.5788037107867,18.0274180093126,
18.7501916019978,19.1988059005238),.UNSPECIFIED.);
#1368=B_SPLINE_CURVE_WITH_KNOTS('',3,(#25096,#25097,#25098,#25099,#25100,
#25101),.UNSPECIFIED.,.F.,.F.,(4,1,1,4),(11.2956184036071,11.744232702133,
12.4670062948183,12.9156205933442),.UNSPECIFIED.);
#1369=B_SPLINE_CURVE_WITH_KNOTS('',3,(#25126,#25127,#25128,#25129,#25130,
#25131),.UNSPECIFIED.,.F.,.F.,(4,1,1,4),(5.0124330964275,5.46104739495341,
6.18382098763867,6.63243528616458),.UNSPECIFIED.);
#1370=B_SPLINE_CURVE_WITH_KNOTS('',3,(#25133,#25134,#25135,#25136,#25137,
#25138,#25139,#25140,#25141,#25142,#25143,#25144,#25145,#25146,#25147,#25148,
#25149,#25150,#25151,#25152,#25153,#25154,#25155,#25156,#25157,#25158,#25159,
#25160,#25161,#25162,#25163,#25164,#25165,#25166,#25167,#25168,#25169,#25170,
#25171,#25172,#25173,#25174,#25175),.UNSPECIFIED.,.F.,.F.,(4,3,3,3,3,3,
3,3,3,3,3,3,3,3,4),(0.,0.0319679902674501,0.0642900427206058,0.0886933568687708,
0.117718239582565,0.124682181362639,0.131745609822757,0.164253554230972,
0.197241305800025,0.230517869135345,0.25235595445092,0.259992045647903,
0.264659623072051,0.29882382302699,0.320892418579125),.UNSPECIFIED.);
#1371=B_SPLINE_CURVE_WITH_KNOTS('',3,(#25180,#25181,#25182,#25183,#25184,
#25185),.UNSPECIFIED.,.F.,.F.,(4,1,1,4),(-3.33195380826789,-2.88333950974197,
-2.16056591705671,-2.06120159751576),.UNSPECIFIED.);
#1372=B_SPLINE_CURVE_WITH_KNOTS('',3,(#25188,#25189,#25190,#25191,#25192,
#25193,#25194,#25195,#25196,#25197,#25198,#25199,#25200,#25201,#25202,#25203,
#25204,#25205,#25206,#25207,#25208,#25209,#25210,#25211,#25212,#25213,#25214,
#25215,#25216,#25217,#25218,#25219,#25220,#25221,#25222,#25223,#25224,#25225,
#25226,#25227,#25228,#25229,#25230,#25231,#25232,#25233,#25234,#25235,#25236,
#25237,#25238,#25239,#25240,#25241,#25242,#25243,#25244,#25245),
 .UNSPECIFIED.,.F.,.F.,(4,3,3,3,3,3,3,3,3,3,3,3,3,3,3,3,3,3,3,4),(-41.0310632895362,
-40.9388473190672,-40.8466422252189,-40.754407737536,-40.6621654402305,
-40.5698612720643,-40.4813266946942,-40.3903969656387,-40.2995162802569,
-40.2086677147606,-40.1178343757824,-40.0269750194882,-39.9361025632024,
-39.8451701195949,-39.8091154310716,-39.7151490717192,-39.6212411951498,
-39.5273766833117,-39.4335563138008,-39.4110634616083),.UNSPECIFIED.);
#1373=B_SPLINE_CURVE_WITH_KNOTS('',3,(#25247,#25248,#25249,#25250,#25251,
#25252),.UNSPECIFIED.,.F.,.F.,(4,1,1,4),(-37.8894729977556,-37.4408586992297,
-36.7180851065444,-36.2694708080185),.UNSPECIFIED.);
#1374=B_SPLINE_CURVE_WITH_KNOTS('',3,(#25254,#25255,#25256,#25257,#25258,
#25259),.UNSPECIFIED.,.F.,.F.,(4,1,1,4),(-34.7478803441658,-34.2992660456399,
-33.5764924529546,-33.1278781544287),.UNSPECIFIED.);
#1375=B_SPLINE_CURVE_WITH_KNOTS('',3,(#25261,#25262,#25263,#25264,#25265,
#25266),.UNSPECIFIED.,.F.,.F.,(4,1,1,4),(-31.606287690576,-31.1576733920501,
-30.4348997993648,-29.9862855008389),.UNSPECIFIED.);
#1376=B_SPLINE_CURVE_WITH_KNOTS('',3,(#25268,#25269,#25270,#25271,#25272,
#25273),.UNSPECIFIED.,.F.,.F.,(4,1,1,4),(-28.4646950369862,-28.0160807384603,
-27.2933071457751,-26.8446928472491),.UNSPECIFIED.);
#1377=B_SPLINE_CURVE_WITH_KNOTS('',3,(#25275,#25276,#25277,#25278,#25279,
#25280),.UNSPECIFIED.,.F.,.F.,(4,1,1,4),(-25.3231023833964,-24.8744880848705,
-24.1517144921853,-23.7031001936593),.UNSPECIFIED.);
#1378=B_SPLINE_CURVE_WITH_KNOTS('',3,(#25282,#25283,#25284,#25285,#25286,
#25287),.UNSPECIFIED.,.F.,.F.,(4,1,1,4),(-22.1815097298066,-21.7328954312807,
-21.0101218385955,-20.5615075400696),.UNSPECIFIED.);
#1379=B_SPLINE_CURVE_WITH_KNOTS('',3,(#25289,#25290,#25291,#25292,#25293,
#25294),.UNSPECIFIED.,.F.,.F.,(4,1,1,4),(-19.0399170762168,-18.5913027776909,
-17.8685291850057,-17.4199148864798),.UNSPECIFIED.);
#1380=B_SPLINE_CURVE_WITH_KNOTS('',3,(#25296,#25297,#25298,#25299,#25300,
#25301),.UNSPECIFIED.,.F.,.F.,(4,1,1,4),(-15.8983244226271,-15.4497101241011,
-14.7269365314159,-14.27832223289),.UNSPECIFIED.);
#1381=B_SPLINE_CURVE_WITH_KNOTS('',3,(#25303,#25304,#25305,#25306,#25307,
#25308),.UNSPECIFIED.,.F.,.F.,(4,1,1,4),(-12.7567317690373,-12.3081174705113,
-11.5853438778261,-11.1367295793002),.UNSPECIFIED.);
#1382=B_SPLINE_CURVE_WITH_KNOTS('',3,(#25310,#25311,#25312,#25313,#25314,
#25315),.UNSPECIFIED.,.F.,.F.,(4,1,1,4),(-9.61513911544747,-9.16652481692155,
-8.4437512242363,-7.99513692571038),.UNSPECIFIED.);
#1383=B_SPLINE_CURVE_WITH_KNOTS('',3,(#25317,#25318,#25319,#25320,#25321,
#25322),.UNSPECIFIED.,.F.,.F.,(4,1,1,4),(-6.47354646185768,-6.02493216333176,
-5.3021585706465,-4.85354427212059),.UNSPECIFIED.);
#1384=B_SPLINE_CURVE_WITH_KNOTS('',3,(#25737,#25738,#25739,#25740,#25741,
#25742,#25743,#25744,#25745,#25746,#25747,#25748,#25749,#25750),
 .UNSPECIFIED.,.F.,.F.,(4,2,2,2,2,2,4),(-0.844212290556731,-0.730966332817565,
-0.619975754240938,-0.457326579004558,-0.29977928179387,-0.147336283383114,
0.),.UNSPECIFIED.);
#1385=B_SPLINE_CURVE_WITH_KNOTS('',3,(#25754,#25755,#25756,#25757,#25758,
#25759,#25760,#25761,#25762,#25763,#25764,#25765,#25766,#25767),
 .UNSPECIFIED.,.F.,.F.,(4,2,2,2,2,2,4),(-0.844212290556731,-0.730966332817565,
-0.619975754240938,-0.457326579004558,-0.29977928179387,-0.147336283383114,
0.),.UNSPECIFIED.);
#1386=B_SPLINE_CURVE_WITH_KNOTS('',3,(#25804,#25805,#25806,#25807,#25808,
#25809,#25810,#25811,#25812,#25813,#25814,#25815,#25816,#25817),
 .UNSPECIFIED.,.F.,.F.,(4,2,2,2,2,2,4),(-0.847325527525843,-0.749719327139836,
-0.649860858750851,-0.495073659399383,-0.335166304629316,-0.170141007879843,
0.),.UNSPECIFIED.);
#1387=B_SPLINE_CURVE_WITH_KNOTS('',3,(#25819,#25820,#25821,#25822,#25823,
#25824,#25825,#25826,#25827,#25828,#25829,#25830,#25831,#25832),
 .UNSPECIFIED.,.F.,.F.,(4,2,2,2,2,2,4),(-0.847325527525843,-0.749719327139836,
-0.649860858750851,-0.495073659399383,-0.335166304629316,-0.170141007879843,
0.),.UNSPECIFIED.);
#1388=B_SPLINE_CURVE_WITH_KNOTS('',3,(#26826,#26827,#26828,#26829,#26830,
#26831,#26832,#26833,#26834,#26835,#26836,#26837,#26838,#26839,#26840,#26841,
#26842,#26843,#26844,#26845,#26846,#26847,#26848,#26849,#26850,#26851,#26852,
#26853,#26854,#26855,#26856,#26857,#26858,#26859,#26860,#26861,#26862,#26863,
#26864,#26865,#26866,#26867,#26868,#26869,#26870,#26871,#26872,#26873,#26874,
#26875,#26876,#26877,#26878,#26879,#26880,#26881,#26882,#26883,#26884,#26885,
#26886,#26887,#26888,#26889,#26890,#26891,#26892,#26893,#26894,#26895,#26896,
#26897,#26898,#26899,#26900,#26901,#26902,#26903,#26904),.UNSPECIFIED.,
 .F.,.F.,(4,1,1,1,1,1,1,1,1,1,1,1,1,1,1,1,1,1,1,1,1,1,1,1,1,1,1,1,1,1,1,
1,1,1,1,1,1,1,1,1,1,1,1,1,1,1,1,1,1,1,1,1,1,1,1,1,1,1,1,1,1,1,1,1,1,1,1,
1,1,1,1,1,1,1,1,1,4),(-37.6991118430775,-37.2030708977739,-36.7070299524702,
-36.2109890071666,-35.7149480618629,-35.2189071165593,-34.7228661712556,
-34.226825225952,-33.7307842806483,-33.2347433353447,-32.738702390041,-32.2426614447374,
-31.7466204994337,-31.25057955413,-30.7545386088264,-30.2584976635227,-29.7624567182191,
-29.2664157729154,-28.7703748276118,-28.2743338823081,-27.7782929370045,
-27.2822519917008,-26.7862110463972,-26.2901701010935,-25.7941291557899,
-25.2980882104862,-24.8020472651826,-24.3060063198789,-23.8099653745753,
-23.3139244292716,-22.817883483968,-22.3218425386643,-21.8258015933607,
-21.329760648057,-20.8337197027534,-20.3376787574497,-19.8416378121461,
-19.3455968668424,-18.8495559215388,-18.3535149762351,-17.8574740309315,
-17.3614330856278,-16.8653921403242,-16.3693511950205,-15.8733102497168,
-15.3772693044132,-14.8812283591095,-14.3851874138059,-13.8891464685022,
-13.3931055231986,-12.8970645778949,-12.4010236325913,-11.9049826872876,
-11.408941741984,-10.9129007966803,-10.4168598513767,-9.92081890607303,
-9.42477796076938,-8.92873701546573,-8.43269607016208,-7.93665512485842,
-7.44061417955477,-6.94457323425112,-6.44853228894747,-5.95249134364382,
-5.45645039834017,-4.96040945303652,-4.46436850773286,-3.96832756242921,
-3.47228661712556,-2.97624567182191,-2.48020472651826,-1.98416378121461,
-1.48812283591095,-0.992081890607303,-0.496040945303652,0.),
 .UNSPECIFIED.);
#1389=B_SPLINE_CURVE_WITH_KNOTS('',3,(#26906,#26907,#26908,#26909,#26910,
#26911,#26912,#26913,#26914,#26915,#26916,#26917,#26918,#26919,#26920,#26921,
#26922,#26923,#26924,#26925),.UNSPECIFIED.,.F.,.F.,(4,2,2,2,2,2,2,2,2,4),
(-0.183449247657807,-0.181303576912795,-0.161079000210457,-0.142089796258872,
-0.119840622322675,-0.0936636492746921,-0.0676644266740556,-0.0408453735972391,
-0.019825886307719,-2.33571946147655E-5),.UNSPECIFIED.);
#1390=B_SPLINE_CURVE_WITH_KNOTS('',3,(#26927,#26928,#26929,#26930,#26931,
#26932,#26933,#26934,#26935,#26936,#26937,#26938,#26939,#26940,#26941,#26942,
#26943,#26944,#26945,#26946,#26947,#26948,#26949,#26950,#26951,#26952,#26953,
#26954,#26955,#26956,#26957,#26958,#26959,#26960,#26961,#26962,#26963,#26964,
#26965,#26966,#26967,#26968,#26969,#26970,#26971,#26972,#26973,#26974,#26975,
#26976,#26977,#26978,#26979,#26980,#26981,#26982,#26983,#26984,#26985,#26986,
#26987,#26988,#26989,#26990,#26991,#26992,#26993,#26994,#26995,#26996,#26997,
#26998,#26999,#27000,#27001,#27002,#27003,#27004,#27005),.UNSPECIFIED.,
 .F.,.F.,(4,1,1,1,1,1,1,1,1,1,1,1,1,1,1,1,1,1,1,1,1,1,1,1,1,1,1,1,1,1,1,
1,1,1,1,1,1,1,1,1,1,1,1,1,1,1,1,1,1,1,1,1,1,1,1,1,1,1,1,1,1,1,1,1,1,1,1,
1,1,1,1,1,1,1,1,1,4),(0.,0.496040945303652,0.992081890607303,1.48812283591095,
1.98416378121461,2.48020472651826,2.97624567182191,3.47228661712556,3.96832756242921,
4.46436850773286,4.96040945303652,5.45645039834017,5.95249134364382,6.44853228894747,
6.94457323425112,7.44061417955477,7.93665512485842,8.43269607016208,8.92873701546573,
9.42477796076938,9.92081890607303,10.4168598513767,10.9129007966803,11.408941741984,
11.9049826872876,12.4010236325913,12.8970645778949,13.3931055231986,13.8891464685022,
14.3851874138059,14.8812283591095,15.3772693044132,15.8733102497168,16.3693511950205,
16.8653921403242,17.3614330856278,17.8574740309315,18.3535149762351,18.8495559215388,
19.3455968668424,19.8416378121461,20.3376787574497,20.8337197027534,21.329760648057,
21.8258015933607,22.3218425386643,22.817883483968,23.3139244292716,23.8099653745753,
24.3060063198789,24.8020472651826,25.2980882104862,25.7941291557899,26.2901701010935,
26.7862110463972,27.2822519917008,27.7782929370045,28.2743338823081,28.7703748276118,
29.2664157729154,29.7624567182191,30.2584976635227,30.7545386088264,31.25057955413,
31.7466204994337,32.2426614447374,32.738702390041,33.2347433353447,33.7307842806483,
34.226825225952,34.7228661712556,35.2189071165593,35.7149480618629,36.2109890071666,
36.7070299524702,37.2030708977739,37.6991118430775),.UNSPECIFIED.);
#1391=B_SPLINE_CURVE_WITH_KNOTS('',3,(#27006,#27007,#27008,#27009,#27010,
#27011,#27012,#27013,#27014,#27015,#27016,#27017,#27018,#27019,#27020,#27021,
#27022,#27023,#27024,#27025),.UNSPECIFIED.,.F.,.F.,(4,2,2,2,2,2,2,2,2,4),
(-0.18344924783076,-0.181303577060204,-0.161079000326594,-0.142089796354812,
-0.119840622394364,-0.0936636493252264,-0.067664426704362,-0.0408453736132039,
-0.0198258863122509,-2.33572184239975E-5),.UNSPECIFIED.);
#1392=B_SPLINE_CURVE_WITH_KNOTS('',3,(#27974,#27975,#27976,#27977,#27978,
#27979,#27980,#27981,#27982,#27983,#27984,#27985,#27986,#27987,#27988,#27989,
#27990,#27991,#27992,#27993,#27994,#27995,#27996),.UNSPECIFIED.,.F.,.F.,
(4,3,2,2,2,2,2,2,2,2,4),(-2.33572184239975E-5,0.,0.011884572475286,0.0237029747818905,
0.0434853822238964,0.0621581371447951,0.0836099647869759,0.108563829632263,
0.134733767979787,0.163062104634996,0.182761473566748),.UNSPECIFIED.);
#1393=B_SPLINE_CURVE_WITH_KNOTS('',3,(#27997,#27998,#27999,#28000,#28001,
#28002,#28003,#28004,#28005,#28006,#28007,#28008,#28009,#28010,#28011,#28012,
#28013,#28014,#28015,#28016,#28017,#28018,#28019),.UNSPECIFIED.,.F.,.F.,
(4,3,2,2,2,2,2,2,2,2,4),(-2.33571946147655E-5,0.,0.0118845724779463,0.0237029747888634,
0.0434853822372858,0.0621581371727652,0.0836099648325251,0.108563829705817,
0.134733768045505,0.163062104655266,0.182761473573992),.UNSPECIFIED.);
#1394=VERTEX_POINT('',#4903);
#1395=VERTEX_POINT('',#4904);
#1396=VERTEX_POINT('',#4941);
#1397=VERTEX_POINT('',#4943);
#1398=VERTEX_POINT('',#4981);
#1399=VERTEX_POINT('',#4983);
#1400=VERTEX_POINT('',#4987);
#1401=VERTEX_POINT('',#4990);
#1402=VERTEX_POINT('',#4992);
#1403=VERTEX_POINT('',#4996);
#1404=VERTEX_POINT('',#5000);
#1405=VERTEX_POINT('',#5004);
#1406=VERTEX_POINT('',#5008);
#1407=VERTEX_POINT('',#5012);
#1408=VERTEX_POINT('',#5016);
#1409=VERTEX_POINT('',#5020);
#1410=VERTEX_POINT('',#5024);
#1411=VERTEX_POINT('',#5028);
#1412=VERTEX_POINT('',#5031);
#1413=VERTEX_POINT('',#5035);
#1414=VERTEX_POINT('',#5038);
#1415=VERTEX_POINT('',#5042);
#1416=VERTEX_POINT('',#5046);
#1417=VERTEX_POINT('',#5050);
#1418=VERTEX_POINT('',#5054);
#1419=VERTEX_POINT('',#5058);
#1420=VERTEX_POINT('',#5061);
#1421=VERTEX_POINT('',#5065);
#1422=VERTEX_POINT('',#5072);
#1423=VERTEX_POINT('',#5073);
#1424=VERTEX_POINT('',#5075);
#1425=VERTEX_POINT('',#5224);
#1426=VERTEX_POINT('',#5232);
#1427=VERTEX_POINT('',#5344);
#1428=VERTEX_POINT('',#5345);
#1429=VERTEX_POINT('',#5541);
#1430=VERTEX_POINT('',#5734);
#1431=VERTEX_POINT('',#5735);
#1432=VERTEX_POINT('',#5737);
#1433=VERTEX_POINT('',#5797);
#1434=VERTEX_POINT('',#5860);
#1435=VERTEX_POINT('',#5861);
#1436=VERTEX_POINT('',#5863);
#1437=VERTEX_POINT('',#6012);
#1438=VERTEX_POINT('',#6171);
#1439=VERTEX_POINT('',#6172);
#1440=VERTEX_POINT('',#6174);
#1441=VERTEX_POINT('',#6559);
#1442=VERTEX_POINT('',#6560);
#1443=VERTEX_POINT('',#6752);
#1444=VERTEX_POINT('',#6958);
#1445=VERTEX_POINT('',#6959);
#1446=VERTEX_POINT('',#6961);
#1447=VERTEX_POINT('',#7345);
#1448=VERTEX_POINT('',#7346);
#1449=VERTEX_POINT('',#7548);
#1450=VERTEX_POINT('',#7746);
#1451=VERTEX_POINT('',#7747);
#1452=VERTEX_POINT('',#7749);
#1453=VERTEX_POINT('',#8141);
#1454=VERTEX_POINT('',#8142);
#1455=VERTEX_POINT('',#8342);
#1456=VERTEX_POINT('',#8550);
#1457=VERTEX_POINT('',#8551);
#1458=VERTEX_POINT('',#8553);
#1459=VERTEX_POINT('',#8953);
#1460=VERTEX_POINT('',#8954);
#1461=VERTEX_POINT('',#9144);
#1462=VERTEX_POINT('',#9335);
#1463=VERTEX_POINT('',#9336);
#1464=VERTEX_POINT('',#9338);
#1465=VERTEX_POINT('',#9394);
#1466=VERTEX_POINT('',#9454);
#1467=VERTEX_POINT('',#9456);
#1468=VERTEX_POINT('',#9457);
#1469=VERTEX_POINT('',#9459);
#1470=VERTEX_POINT('',#9466);
#1471=VERTEX_POINT('',#9657);
#1472=VERTEX_POINT('',#9848);
#1473=VERTEX_POINT('',#10039);
#1474=VERTEX_POINT('',#10230);
#1475=VERTEX_POINT('',#10421);
#1476=VERTEX_POINT('',#10612);
#1477=VERTEX_POINT('',#10803);
#1478=VERTEX_POINT('',#10994);
#1479=VERTEX_POINT('',#11185);
#1480=VERTEX_POINT('',#11376);
#1481=VERTEX_POINT('',#11570);
#1482=VERTEX_POINT('',#11761);
#1483=VERTEX_POINT('',#11772);
#1484=VERTEX_POINT('',#11774);
#1485=VERTEX_POINT('',#11784);
#1486=VERTEX_POINT('',#11978);
#1487=VERTEX_POINT('',#12169);
#1488=VERTEX_POINT('',#12360);
#1489=VERTEX_POINT('',#12551);
#1490=VERTEX_POINT('',#12745);
#1491=VERTEX_POINT('',#12936);
#1492=VERTEX_POINT('',#13127);
#1493=VERTEX_POINT('',#13318);
#1494=VERTEX_POINT('',#13509);
#1495=VERTEX_POINT('',#13700);
#1496=VERTEX_POINT('',#13891);
#1497=VERTEX_POINT('',#14082);
#1498=VERTEX_POINT('',#14185);
#1499=VERTEX_POINT('',#14191);
#1500=VERTEX_POINT('',#14283);
#1501=VERTEX_POINT('',#14285);
#1502=VERTEX_POINT('',#14345);
#1503=VERTEX_POINT('',#14347);
#1504=VERTEX_POINT('',#14350);
#1505=VERTEX_POINT('',#14352);
#1506=VERTEX_POINT('',#14356);
#1507=VERTEX_POINT('',#14362);
#1508=VERTEX_POINT('',#15422);
#1509=VERTEX_POINT('',#15424);
#1510=VERTEX_POINT('',#15428);
#1511=VERTEX_POINT('',#15433);
#1512=VERTEX_POINT('',#15435);
#1513=VERTEX_POINT('',#15439);
#1514=VERTEX_POINT('',#15444);
#1515=VERTEX_POINT('',#15448);
#1516=VERTEX_POINT('',#15451);
#1517=VERTEX_POINT('',#15453);
#1518=VERTEX_POINT('',#15457);
#1519=VERTEX_POINT('',#15461);
#1520=VERTEX_POINT('',#15466);
#1521=VERTEX_POINT('',#15470);
#1522=VERTEX_POINT('',#15474);
#1523=VERTEX_POINT('',#15478);
#1524=VERTEX_POINT('',#15481);
#1525=VERTEX_POINT('',#15483);
#1526=VERTEX_POINT('',#15487);
#1527=VERTEX_POINT('',#15491);
#1528=VERTEX_POINT('',#15494);
#1529=VERTEX_POINT('',#15498);
#1530=VERTEX_POINT('',#15501);
#1531=VERTEX_POINT('',#15503);
#1532=VERTEX_POINT('',#15542);
#1533=VERTEX_POINT('',#15543);
#1534=VERTEX_POINT('',#15558);
#1535=VERTEX_POINT('',#15560);
#1536=VERTEX_POINT('',#15577);
#1537=VERTEX_POINT('',#15579);
#1538=VERTEX_POINT('',#15610);
#1539=VERTEX_POINT('',#15625);
#1540=VERTEX_POINT('',#15645);
#1541=VERTEX_POINT('',#15646);
#1542=VERTEX_POINT('',#15648);
#1543=VERTEX_POINT('',#15650);
#1544=VERTEX_POINT('',#15654);
#1545=VERTEX_POINT('',#15656);
#1546=VERTEX_POINT('',#15660);
#1547=VERTEX_POINT('',#15662);
#1548=VERTEX_POINT('',#15666);
#1549=VERTEX_POINT('',#15668);
#1550=VERTEX_POINT('',#15672);
#1551=VERTEX_POINT('',#15674);
#1552=VERTEX_POINT('',#15684);
#1553=VERTEX_POINT('',#15685);
#1554=VERTEX_POINT('',#15687);
#1555=VERTEX_POINT('',#15842);
#1556=VERTEX_POINT('',#15957);
#1557=VERTEX_POINT('',#15958);
#1558=VERTEX_POINT('',#15960);
#1559=VERTEX_POINT('',#16176);
#1560=VERTEX_POINT('',#16350);
#1561=VERTEX_POINT('',#16351);
#1562=VERTEX_POINT('',#16353);
#1563=VERTEX_POINT('',#16709);
#1564=VERTEX_POINT('',#16710);
#1565=VERTEX_POINT('',#16882);
#1566=VERTEX_POINT('',#17050);
#1567=VERTEX_POINT('',#17051);
#1568=VERTEX_POINT('',#17053);
#1569=VERTEX_POINT('',#17393);
#1570=VERTEX_POINT('',#17394);
#1571=VERTEX_POINT('',#17566);
#1572=VERTEX_POINT('',#17781);
#1573=VERTEX_POINT('',#17782);
#1574=VERTEX_POINT('',#17859);
#1575=VERTEX_POINT('',#17861);
#1576=VERTEX_POINT('',#17899);
#1577=VERTEX_POINT('',#18129);
#1578=VERTEX_POINT('',#18362);
#1579=VERTEX_POINT('',#18592);
#1580=VERTEX_POINT('',#18603);
#1581=VERTEX_POINT('',#18833);
#1582=VERTEX_POINT('',#19066);
#1583=VERTEX_POINT('',#19119);
#1584=VERTEX_POINT('',#19121);
#1585=VERTEX_POINT('',#19126);
#1586=VERTEX_POINT('',#19362);
#1587=VERTEX_POINT('',#19592);
#1588=VERTEX_POINT('',#19825);
#1589=VERTEX_POINT('',#20058);
#1590=VERTEX_POINT('',#20521);
#1591=VERTEX_POINT('',#20550);
#1592=VERTEX_POINT('',#20711);
#1593=VERTEX_POINT('',#20713);
#1594=VERTEX_POINT('',#20878);
#1595=VERTEX_POINT('',#20879);
#1596=VERTEX_POINT('',#20968);
#1597=VERTEX_POINT('',#20973);
#1598=VERTEX_POINT('',#21088);
#1599=VERTEX_POINT('',#21090);
#1600=VERTEX_POINT('',#21141);
#1601=VERTEX_POINT('',#21230);
#1602=VERTEX_POINT('',#21321);
#1603=VERTEX_POINT('',#21325);
#1604=VERTEX_POINT('',#22111);
#1605=VERTEX_POINT('',#22113);
#1606=VERTEX_POINT('',#22121);
#1607=VERTEX_POINT('',#22123);
#1608=VERTEX_POINT('',#22127);
#1609=VERTEX_POINT('',#22132);
#1610=VERTEX_POINT('',#22138);
#1611=VERTEX_POINT('',#22140);
#1612=VERTEX_POINT('',#22144);
#1613=VERTEX_POINT('',#22149);
#1614=VERTEX_POINT('',#22155);
#1615=VERTEX_POINT('',#22156);
#1616=VERTEX_POINT('',#22165);
#1617=VERTEX_POINT('',#22167);
#1618=VERTEX_POINT('',#22174);
#1619=VERTEX_POINT('',#22176);
#1620=VERTEX_POINT('',#22185);
#1621=VERTEX_POINT('',#22187);
#1622=VERTEX_POINT('',#22196);
#1623=VERTEX_POINT('',#22198);
#1624=VERTEX_POINT('',#22207);
#1625=VERTEX_POINT('',#22209);
#1626=VERTEX_POINT('',#22218);
#1627=VERTEX_POINT('',#22220);
#1628=VERTEX_POINT('',#22229);
#1629=VERTEX_POINT('',#22231);
#1630=VERTEX_POINT('',#22240);
#1631=VERTEX_POINT('',#22242);
#1632=VERTEX_POINT('',#22251);
#1633=VERTEX_POINT('',#22253);
#1634=VERTEX_POINT('',#22262);
#1635=VERTEX_POINT('',#22264);
#1636=VERTEX_POINT('',#22273);
#1637=VERTEX_POINT('',#22275);
#1638=VERTEX_POINT('',#22284);
#1639=VERTEX_POINT('',#22286);
#1640=VERTEX_POINT('',#22295);
#1641=VERTEX_POINT('',#22297);
#1642=VERTEX_POINT('',#22306);
#1643=VERTEX_POINT('',#22308);
#1644=VERTEX_POINT('',#22310);
#1645=VERTEX_POINT('',#22317);
#1646=VERTEX_POINT('',#22319);
#1647=VERTEX_POINT('',#22328);
#1648=VERTEX_POINT('',#22330);
#1649=VERTEX_POINT('',#22339);
#1650=VERTEX_POINT('',#22341);
#1651=VERTEX_POINT('',#22350);
#1652=VERTEX_POINT('',#22352);
#1653=VERTEX_POINT('',#22361);
#1654=VERTEX_POINT('',#22363);
#1655=VERTEX_POINT('',#22372);
#1656=VERTEX_POINT('',#22374);
#1657=VERTEX_POINT('',#22383);
#1658=VERTEX_POINT('',#22385);
#1659=VERTEX_POINT('',#22394);
#1660=VERTEX_POINT('',#22396);
#1661=VERTEX_POINT('',#22405);
#1662=VERTEX_POINT('',#22407);
#1663=VERTEX_POINT('',#22416);
#1664=VERTEX_POINT('',#22418);
#1665=VERTEX_POINT('',#22427);
#1666=VERTEX_POINT('',#22429);
#1667=VERTEX_POINT('',#22438);
#1668=VERTEX_POINT('',#22440);
#1669=VERTEX_POINT('',#22451);
#1670=VERTEX_POINT('',#22452);
#1671=VERTEX_POINT('',#22459);
#1672=VERTEX_POINT('',#22461);
#1673=VERTEX_POINT('',#22470);
#1674=VERTEX_POINT('',#22472);
#1675=VERTEX_POINT('',#22481);
#1676=VERTEX_POINT('',#22483);
#1677=VERTEX_POINT('',#22492);
#1678=VERTEX_POINT('',#22494);
#1679=VERTEX_POINT('',#22503);
#1680=VERTEX_POINT('',#22505);
#1681=VERTEX_POINT('',#22514);
#1682=VERTEX_POINT('',#22516);
#1683=VERTEX_POINT('',#22525);
#1684=VERTEX_POINT('',#22527);
#1685=VERTEX_POINT('',#22536);
#1686=VERTEX_POINT('',#22538);
#1687=VERTEX_POINT('',#22547);
#1688=VERTEX_POINT('',#22549);
#1689=VERTEX_POINT('',#22558);
#1690=VERTEX_POINT('',#22560);
#1691=VERTEX_POINT('',#22569);
#1692=VERTEX_POINT('',#22571);
#1693=VERTEX_POINT('',#22580);
#1694=VERTEX_POINT('',#22582);
#1695=VERTEX_POINT('',#22591);
#1696=VERTEX_POINT('',#22593);
#1697=VERTEX_POINT('',#22595);
#1698=VERTEX_POINT('',#22602);
#1699=VERTEX_POINT('',#22604);
#1700=VERTEX_POINT('',#22613);
#1701=VERTEX_POINT('',#22615);
#1702=VERTEX_POINT('',#22624);
#1703=VERTEX_POINT('',#22626);
#1704=VERTEX_POINT('',#22635);
#1705=VERTEX_POINT('',#22637);
#1706=VERTEX_POINT('',#22646);
#1707=VERTEX_POINT('',#22648);
#1708=VERTEX_POINT('',#22657);
#1709=VERTEX_POINT('',#22659);
#1710=VERTEX_POINT('',#22668);
#1711=VERTEX_POINT('',#22670);
#1712=VERTEX_POINT('',#22679);
#1713=VERTEX_POINT('',#22681);
#1714=VERTEX_POINT('',#22690);
#1715=VERTEX_POINT('',#22692);
#1716=VERTEX_POINT('',#22701);
#1717=VERTEX_POINT('',#22703);
#1718=VERTEX_POINT('',#22712);
#1719=VERTEX_POINT('',#22714);
#1720=VERTEX_POINT('',#22723);
#1721=VERTEX_POINT('',#22725);
#1722=VERTEX_POINT('',#22734);
#1723=VERTEX_POINT('',#22736);
#1724=VERTEX_POINT('',#22747);
#1725=VERTEX_POINT('',#24551);
#1726=VERTEX_POINT('',#24610);
#1727=VERTEX_POINT('',#24634);
#1728=VERTEX_POINT('',#24664);
#1729=VERTEX_POINT('',#25179);
#1730=VERTEX_POINT('',#25654);
#1731=VERTEX_POINT('',#25656);
#1732=VERTEX_POINT('',#25663);
#1733=VERTEX_POINT('',#25665);
#1734=VERTEX_POINT('',#25669);
#1735=VERTEX_POINT('',#25674);
#1736=VERTEX_POINT('',#25676);
#1737=VERTEX_POINT('',#25680);
#1738=VERTEX_POINT('',#25685);
#1739=VERTEX_POINT('',#25687);
#1740=VERTEX_POINT('',#25691);
#1741=VERTEX_POINT('',#25693);
#1742=VERTEX_POINT('',#25698);
#1743=VERTEX_POINT('',#25702);
#1744=VERTEX_POINT('',#25735);
#1745=VERTEX_POINT('',#25736);
#1746=VERTEX_POINT('',#25751);
#1747=VERTEX_POINT('',#25753);
#1748=VERTEX_POINT('',#25770);
#1749=VERTEX_POINT('',#25772);
#1750=VERTEX_POINT('',#25803);
#1751=VERTEX_POINT('',#25818);
#1752=VERTEX_POINT('',#25838);
#1753=VERTEX_POINT('',#25839);
#1754=VERTEX_POINT('',#25841);
#1755=VERTEX_POINT('',#25843);
#1756=VERTEX_POINT('',#25847);
#1757=VERTEX_POINT('',#25849);
#1758=VERTEX_POINT('',#25853);
#1759=VERTEX_POINT('',#25855);
#1760=VERTEX_POINT('',#25859);
#1761=VERTEX_POINT('',#25861);
#1762=VERTEX_POINT('',#25865);
#1763=VERTEX_POINT('',#25867);
#1764=VERTEX_POINT('',#26824);
#1765=VERTEX_POINT('',#26825);
#1766=VERTEX_POINT('',#26905);
#1767=VERTEX_POINT('',#26926);
#1768=EDGE_CURVE('',#1394,#1395,#1137,.T.);
#1769=EDGE_CURVE('',#1395,#1394,#1138,.T.);
#1770=EDGE_CURVE('',#1395,#1396,#821,.T.);
#1771=EDGE_CURVE('',#1397,#1396,#1139,.T.);
#1772=EDGE_CURVE('',#1396,#1397,#1140,.T.);
#1773=EDGE_CURVE('',#1398,#1398,#256,.T.);
#1774=EDGE_CURVE('',#1398,#1399,#822,.T.);
#1775=EDGE_CURVE('',#1399,#1399,#257,.T.);
#1776=EDGE_CURVE('',#1400,#1400,#258,.T.);
#1777=EDGE_CURVE('',#1401,#1401,#259,.T.);
#1778=EDGE_CURVE('',#1401,#1402,#823,.T.);
#1779=EDGE_CURVE('',#1402,#1402,#260,.T.);
#1780=EDGE_CURVE('',#1403,#1403,#261,.T.);
#1781=EDGE_CURVE('',#1403,#1401,#824,.T.);
#1782=EDGE_CURVE('',#1403,#1404,#825,.T.);
#1783=EDGE_CURVE('',#1404,#1404,#262,.T.);
#1784=EDGE_CURVE('',#1405,#1405,#263,.T.);
#1785=EDGE_CURVE('',#1405,#1404,#826,.T.);
#1786=EDGE_CURVE('',#1406,#1406,#264,.T.);
#1787=EDGE_CURVE('',#1406,#1405,#827,.T.);
#1788=EDGE_CURVE('',#1406,#1407,#828,.T.);
#1789=EDGE_CURVE('',#1407,#1407,#265,.T.);
#1790=EDGE_CURVE('',#1408,#1408,#266,.T.);
#1791=EDGE_CURVE('',#1408,#1407,#829,.T.);
#1792=EDGE_CURVE('',#1409,#1409,#267,.T.);
#1793=EDGE_CURVE('',#1409,#1408,#830,.T.);
#1794=EDGE_CURVE('',#1410,#1410,#268,.T.);
#1795=EDGE_CURVE('',#1410,#1409,#831,.T.);
#1796=EDGE_CURVE('',#1411,#1411,#269,.T.);
#1797=EDGE_CURVE('',#1412,#1412,#270,.T.);
#1798=EDGE_CURVE('',#1412,#1411,#832,.T.);
#1799=EDGE_CURVE('',#1413,#1413,#271,.T.);
#1800=EDGE_CURVE('',#1414,#1414,#272,.T.);
#1801=EDGE_CURVE('',#1414,#1413,#833,.T.);
#1802=EDGE_CURVE('',#1415,#1415,#273,.T.);
#1803=EDGE_CURVE('',#1415,#1414,#834,.T.);
#1804=EDGE_CURVE('',#1416,#1416,#274,.T.);
#1805=EDGE_CURVE('',#1416,#1415,#835,.T.);
#1806=EDGE_CURVE('',#1417,#1417,#275,.T.);
#1807=EDGE_CURVE('',#1417,#1416,#836,.T.);
#1808=EDGE_CURVE('',#1418,#1418,#276,.T.);
#1809=EDGE_CURVE('',#1418,#1417,#837,.T.);
#1810=EDGE_CURVE('',#1419,#1419,#277,.T.);
#1811=EDGE_CURVE('',#1420,#1420,#278,.T.);
#1812=EDGE_CURVE('',#1420,#1419,#838,.T.);
#1813=EDGE_CURVE('',#1421,#1421,#279,.T.);
#1814=EDGE_CURVE('',#1400,#1421,#839,.T.);
#1815=EDGE_CURVE('',#1422,#1423,#840,.T.);
#1816=EDGE_CURVE('',#1424,#1422,#1141,.F.);
#1817=EDGE_CURVE('',#1425,#1424,#1142,.T.);
#1818=EDGE_CURVE('',#1426,#1425,#280,.T.);
#1819=EDGE_CURVE('',#1426,#1423,#1143,.T.);
#1820=EDGE_CURVE('',#1427,#1428,#841,.T.);
#1821=EDGE_CURVE('',#1422,#1427,#1144,.F.);
#1822=EDGE_CURVE('',#1423,#1429,#1145,.T.);
#1823=EDGE_CURVE('',#1429,#1428,#1146,.T.);
#1824=EDGE_CURVE('',#1430,#1431,#842,.T.);
#1825=EDGE_CURVE('',#1432,#1430,#1147,.T.);
#1826=EDGE_CURVE('',#1427,#1432,#1148,.F.);
#1827=EDGE_CURVE('',#1428,#1433,#1149,.T.);
#1828=EDGE_CURVE('',#1433,#1431,#1150,.T.);
#1829=EDGE_CURVE('',#1434,#1435,#843,.T.);
#1830=EDGE_CURVE('',#1436,#1434,#1151,.T.);
#1831=EDGE_CURVE('',#1430,#1436,#1152,.T.);
#1832=EDGE_CURVE('',#1431,#1437,#1153,.T.);
#1833=EDGE_CURVE('',#1437,#1435,#1154,.T.);
#1834=EDGE_CURVE('',#1438,#1439,#844,.T.);
#1835=EDGE_CURVE('',#1440,#1438,#1155,.F.);
#1836=EDGE_CURVE('',#1434,#1440,#1156,.T.);
#1837=EDGE_CURVE('',#1435,#1439,#1157,.T.);
#1838=EDGE_CURVE('',#1441,#1442,#845,.T.);
#1839=EDGE_CURVE('',#1438,#1441,#1158,.F.);
#1840=EDGE_CURVE('',#1439,#1443,#1159,.T.);
#1841=EDGE_CURVE('',#1443,#1442,#1160,.T.);
#1842=EDGE_CURVE('',#1444,#1445,#846,.T.);
#1843=EDGE_CURVE('',#1446,#1444,#1161,.F.);
#1844=EDGE_CURVE('',#1441,#1446,#1162,.F.);
#1845=EDGE_CURVE('',#1442,#1445,#1163,.T.);
#1846=EDGE_CURVE('',#1447,#1448,#847,.T.);
#1847=EDGE_CURVE('',#1444,#1447,#1164,.F.);
#1848=EDGE_CURVE('',#1445,#1449,#1165,.T.);
#1849=EDGE_CURVE('',#1449,#1448,#1166,.T.);
#1850=EDGE_CURVE('',#1450,#1451,#848,.T.);
#1851=EDGE_CURVE('',#1452,#1450,#1167,.F.);
#1852=EDGE_CURVE('',#1447,#1452,#1168,.F.);
#1853=EDGE_CURVE('',#1448,#1451,#1169,.T.);
#1854=EDGE_CURVE('',#1453,#1454,#849,.T.);
#1855=EDGE_CURVE('',#1450,#1453,#1170,.F.);
#1856=EDGE_CURVE('',#1451,#1455,#1171,.T.);
#1857=EDGE_CURVE('',#1455,#1454,#1172,.T.);
#1858=EDGE_CURVE('',#1456,#1457,#850,.T.);
#1859=EDGE_CURVE('',#1458,#1456,#1173,.F.);
#1860=EDGE_CURVE('',#1453,#1458,#1174,.F.);
#1861=EDGE_CURVE('',#1454,#1457,#1175,.T.);
#1862=EDGE_CURVE('',#1459,#1460,#851,.T.);
#1863=EDGE_CURVE('',#1456,#1459,#1176,.F.);
#1864=EDGE_CURVE('',#1457,#1461,#1177,.T.);
#1865=EDGE_CURVE('',#1461,#1460,#1178,.T.);
#1866=EDGE_CURVE('',#1462,#1463,#852,.T.);
#1867=EDGE_CURVE('',#1464,#1462,#1179,.T.);
#1868=EDGE_CURVE('',#1459,#1464,#1180,.F.);
#1869=EDGE_CURVE('',#1460,#1465,#1181,.T.);
#1870=EDGE_CURVE('',#1465,#1463,#1182,.T.);
#1871=EDGE_CURVE('',#1466,#1466,#281,.F.);
#1872=EDGE_CURVE('',#1467,#1468,#282,.T.);
#1873=EDGE_CURVE('',#1468,#1469,#1183,.T.);
#1874=EDGE_CURVE('',#1469,#1470,#1184,.T.);
#1875=EDGE_CURVE('',#1470,#1471,#1185,.T.);
#1876=EDGE_CURVE('',#1471,#1472,#1186,.T.);
#1877=EDGE_CURVE('',#1472,#1473,#1187,.T.);
#1878=EDGE_CURVE('',#1473,#1474,#1188,.T.);
#1879=EDGE_CURVE('',#1474,#1475,#1189,.T.);
#1880=EDGE_CURVE('',#1475,#1476,#1190,.T.);
#1881=EDGE_CURVE('',#1476,#1477,#1191,.T.);
#1882=EDGE_CURVE('',#1477,#1478,#1192,.T.);
#1883=EDGE_CURVE('',#1478,#1479,#1193,.T.);
#1884=EDGE_CURVE('',#1479,#1480,#1194,.T.);
#1885=EDGE_CURVE('',#1480,#1481,#1195,.T.);
#1886=EDGE_CURVE('',#1481,#1482,#1196,.T.);
#1887=EDGE_CURVE('',#1483,#1482,#283,.F.);
#1888=EDGE_CURVE('',#1483,#1484,#1197,.T.);
#1889=EDGE_CURVE('',#1484,#1485,#1198,.T.);
#1890=EDGE_CURVE('',#1485,#1486,#1199,.T.);
#1891=EDGE_CURVE('',#1486,#1487,#1200,.T.);
#1892=EDGE_CURVE('',#1487,#1488,#1201,.T.);
#1893=EDGE_CURVE('',#1488,#1489,#1202,.T.);
#1894=EDGE_CURVE('',#1489,#1490,#1203,.T.);
#1895=EDGE_CURVE('',#1490,#1491,#1204,.T.);
#1896=EDGE_CURVE('',#1491,#1492,#1205,.T.);
#1897=EDGE_CURVE('',#1492,#1493,#1206,.T.);
#1898=EDGE_CURVE('',#1493,#1494,#1207,.T.);
#1899=EDGE_CURVE('',#1494,#1495,#1208,.T.);
#1900=EDGE_CURVE('',#1495,#1496,#1209,.T.);
#1901=EDGE_CURVE('',#1496,#1497,#1210,.T.);
#1902=EDGE_CURVE('',#1497,#1467,#1211,.T.);
#1903=EDGE_CURVE('',#1463,#1498,#1212,.T.);
#1904=EDGE_CURVE('',#1498,#1499,#1213,.T.);
#1905=EDGE_CURVE('',#1500,#1499,#284,.T.);
#1906=EDGE_CURVE('',#1501,#1500,#1214,.T.);
#1907=EDGE_CURVE('',#1462,#1501,#1215,.T.);
#1908=EDGE_CURVE('',#1502,#1502,#285,.T.);
#1909=EDGE_CURVE('',#1503,#1503,#286,.T.);
#1910=EDGE_CURVE('',#1504,#1504,#287,.T.);
#1911=EDGE_CURVE('',#1504,#1505,#288,.T.);
#1912=EDGE_CURVE('',#1505,#1505,#289,.T.);
#1913=EDGE_CURVE('',#1505,#1506,#853,.T.);
#1914=EDGE_CURVE('',#1506,#1506,#290,.T.);
#1915=EDGE_CURVE('',#1506,#1502,#291,.T.);
#1916=EDGE_CURVE('',#1507,#1507,#292,.T.);
#1917=EDGE_CURVE('',#1482,#1500,#1216,.T.);
#1918=EDGE_CURVE('',#1425,#1468,#1217,.T.);
#1919=EDGE_CURVE('',#1467,#1426,#1218,.T.);
#1920=EDGE_CURVE('',#1499,#1483,#1219,.T.);
#1921=EDGE_CURVE('',#1508,#1508,#293,.T.);
#1922=EDGE_CURVE('',#1508,#1509,#294,.T.);
#1923=EDGE_CURVE('',#1509,#1509,#295,.T.);
#1924=EDGE_CURVE('',#1509,#1510,#854,.T.);
#1925=EDGE_CURVE('',#1510,#1510,#296,.T.);
#1926=EDGE_CURVE('',#1511,#1511,#297,.T.);
#1927=EDGE_CURVE('',#1511,#1512,#298,.T.);
#1928=EDGE_CURVE('',#1512,#1512,#299,.T.);
#1929=EDGE_CURVE('',#1512,#1513,#855,.T.);
#1930=EDGE_CURVE('',#1513,#1513,#300,.T.);
#1931=EDGE_CURVE('',#1513,#1514,#301,.T.);
#1932=EDGE_CURVE('',#1514,#1514,#302,.T.);
#1933=EDGE_CURVE('',#1515,#1515,#303,.T.);
#1934=EDGE_CURVE('',#1516,#1516,#304,.T.);
#1935=EDGE_CURVE('',#1516,#1517,#305,.T.);
#1936=EDGE_CURVE('',#1517,#1517,#306,.T.);
#1937=EDGE_CURVE('',#1517,#1518,#856,.T.);
#1938=EDGE_CURVE('',#1518,#1518,#307,.T.);
#1939=EDGE_CURVE('',#1519,#1519,#308,.T.);
#1940=EDGE_CURVE('',#1518,#1507,#309,.T.);
#1941=EDGE_CURVE('',#1503,#1520,#310,.T.);
#1942=EDGE_CURVE('',#1520,#1520,#311,.T.);
#1943=EDGE_CURVE('',#1520,#1521,#857,.T.);
#1944=EDGE_CURVE('',#1521,#1521,#312,.T.);
#1945=EDGE_CURVE('',#1521,#1522,#313,.T.);
#1946=EDGE_CURVE('',#1522,#1522,#314,.T.);
#1947=EDGE_CURVE('',#1523,#1523,#315,.T.);
#1948=EDGE_CURVE('',#1524,#1524,#316,.T.);
#1949=EDGE_CURVE('',#1524,#1525,#317,.T.);
#1950=EDGE_CURVE('',#1525,#1525,#318,.T.);
#1951=EDGE_CURVE('',#1525,#1526,#858,.T.);
#1952=EDGE_CURVE('',#1526,#1526,#319,.T.);
#1953=EDGE_CURVE('',#1527,#1527,#320,.T.);
#1954=EDGE_CURVE('',#1526,#1528,#321,.T.);
#1955=EDGE_CURVE('',#1528,#1528,#322,.T.);
#1956=EDGE_CURVE('',#1529,#1529,#323,.T.);
#1957=EDGE_CURVE('',#1530,#1530,#324,.T.);
#1958=EDGE_CURVE('',#1530,#1531,#325,.T.);
#1959=EDGE_CURVE('',#1531,#1531,#326,.T.);
#1960=EDGE_CURVE('',#1529,#1530,#859,.T.);
#1961=EDGE_CURVE('',#1523,#1527,#860,.T.);
#1962=EDGE_CURVE('',#1515,#1519,#861,.T.);
#1963=EDGE_CURVE('',#1532,#1533,#1220,.T.);
#1964=EDGE_CURVE('',#1533,#1534,#862,.T.);
#1965=EDGE_CURVE('',#1535,#1534,#1221,.T.);
#1966=EDGE_CURVE('',#1532,#1535,#863,.T.);
#1967=EDGE_CURVE('',#1536,#1532,#327,.T.);
#1968=EDGE_CURVE('',#1537,#1535,#328,.T.);
#1969=EDGE_CURVE('',#1536,#1537,#864,.T.);
#1970=EDGE_CURVE('',#1538,#1536,#1222,.T.);
#1971=EDGE_CURVE('',#1539,#1537,#1223,.T.);
#1972=EDGE_CURVE('',#1538,#1539,#865,.T.);
#1973=EDGE_CURVE('',#1533,#1538,#329,.T.);
#1974=EDGE_CURVE('',#1534,#1539,#330,.T.);
#1975=EDGE_CURVE('',#1540,#1541,#866,.T.);
#1976=EDGE_CURVE('',#1541,#1542,#867,.T.);
#1977=EDGE_CURVE('',#1543,#1542,#868,.T.);
#1978=EDGE_CURVE('',#1540,#1543,#869,.T.);
#1979=EDGE_CURVE('',#1544,#1540,#870,.T.);
#1980=EDGE_CURVE('',#1545,#1543,#871,.T.);
#1981=EDGE_CURVE('',#1544,#1545,#872,.T.);
#1982=EDGE_CURVE('',#1546,#1544,#873,.T.);
#1983=EDGE_CURVE('',#1547,#1545,#874,.T.);
#1984=EDGE_CURVE('',#1546,#1547,#875,.T.);
#1985=EDGE_CURVE('',#1548,#1546,#876,.T.);
#1986=EDGE_CURVE('',#1549,#1547,#877,.T.);
#1987=EDGE_CURVE('',#1548,#1549,#878,.T.);
#1988=EDGE_CURVE('',#1550,#1548,#879,.T.);
#1989=EDGE_CURVE('',#1551,#1549,#880,.T.);
#1990=EDGE_CURVE('',#1550,#1551,#881,.T.);
#1991=EDGE_CURVE('',#1541,#1550,#882,.T.);
#1992=EDGE_CURVE('',#1542,#1551,#883,.T.);
#1993=EDGE_CURVE('',#1552,#1553,#884,.T.);
#1994=EDGE_CURVE('',#1554,#1552,#1224,.T.);
#1995=EDGE_CURVE('',#1555,#1554,#331,.T.);
#1996=EDGE_CURVE('',#1555,#1553,#1225,.T.);
#1997=EDGE_CURVE('',#1556,#1557,#885,.T.);
#1998=EDGE_CURVE('',#1558,#1556,#1226,.T.);
#1999=EDGE_CURVE('',#1552,#1558,#1227,.T.);
#2000=EDGE_CURVE('',#1553,#1559,#1228,.T.);
#2001=EDGE_CURVE('',#1559,#1557,#1229,.T.);
#2002=EDGE_CURVE('',#1560,#1561,#886,.T.);
#2003=EDGE_CURVE('',#1562,#1560,#1230,.F.);
#2004=EDGE_CURVE('',#1556,#1562,#1231,.T.);
#2005=EDGE_CURVE('',#1557,#1561,#1232,.T.);
#2006=EDGE_CURVE('',#1563,#1564,#887,.T.);
#2007=EDGE_CURVE('',#1560,#1563,#1233,.F.);
#2008=EDGE_CURVE('',#1561,#1565,#1234,.T.);
#2009=EDGE_CURVE('',#1565,#1564,#1235,.T.);
#2010=EDGE_CURVE('',#1566,#1567,#888,.T.);
#2011=EDGE_CURVE('',#1568,#1566,#1236,.F.);
#2012=EDGE_CURVE('',#1563,#1568,#1237,.F.);
#2013=EDGE_CURVE('',#1564,#1567,#1238,.T.);
#2014=EDGE_CURVE('',#1569,#1570,#889,.T.);
#2015=EDGE_CURVE('',#1566,#1569,#1239,.F.);
#2016=EDGE_CURVE('',#1567,#1571,#1240,.T.);
#2017=EDGE_CURVE('',#1571,#1570,#1241,.T.);
#2018=EDGE_CURVE('',#1572,#1573,#1242,.T.);
#2019=EDGE_CURVE('',#1573,#1574,#332,.F.);
#2020=EDGE_CURVE('',#1574,#1575,#1243,.T.);
#2021=EDGE_CURVE('',#1575,#1576,#1244,.T.);
#2022=EDGE_CURVE('',#1576,#1577,#1245,.T.);
#2023=EDGE_CURVE('',#1577,#1578,#1246,.T.);
#2024=EDGE_CURVE('',#1578,#1579,#1247,.T.);
#2025=EDGE_CURVE('',#1579,#1580,#1248,.T.);
#2026=EDGE_CURVE('',#1580,#1581,#1249,.T.);
#2027=EDGE_CURVE('',#1581,#1582,#1250,.T.);
#2028=EDGE_CURVE('',#1583,#1582,#333,.F.);
#2029=EDGE_CURVE('',#1583,#1584,#1251,.T.);
#2030=EDGE_CURVE('',#1584,#1585,#1252,.T.);
#2031=EDGE_CURVE('',#1585,#1586,#1253,.T.);
#2032=EDGE_CURVE('',#1586,#1587,#1254,.T.);
#2033=EDGE_CURVE('',#1587,#1588,#1255,.T.);
#2034=EDGE_CURVE('',#1588,#1589,#1256,.T.);
#2035=EDGE_CURVE('',#1589,#1572,#1257,.T.);
#2036=EDGE_CURVE('',#1570,#1590,#1258,.T.);
#2037=EDGE_CURVE('',#1590,#1591,#1259,.T.);
#2038=EDGE_CURVE('',#1592,#1591,#334,.T.);
#2039=EDGE_CURVE('',#1593,#1592,#1260,.T.);
#2040=EDGE_CURVE('',#1569,#1593,#1261,.F.);
#2041=EDGE_CURVE('',#1594,#1595,#1262,.T.);
#2042=EDGE_CURVE('',#1594,#1596,#1263,.T.);
#2043=EDGE_CURVE('',#1596,#1597,#1264,.T.);
#2044=EDGE_CURVE('',#1597,#1595,#1265,.T.);
#2045=EDGE_CURVE('',#1595,#1598,#335,.T.);
#2046=EDGE_CURVE('',#1597,#1599,#336,.T.);
#2047=EDGE_CURVE('',#1599,#1598,#1266,.T.);
#2048=EDGE_CURVE('',#1598,#1600,#1267,.T.);
#2049=EDGE_CURVE('',#1599,#1601,#1268,.T.);
#2050=EDGE_CURVE('',#1601,#1600,#1269,.T.);
#2051=EDGE_CURVE('',#1596,#1602,#337,.T.);
#2052=EDGE_CURVE('',#1602,#1601,#338,.T.);
#2053=EDGE_CURVE('',#1603,#1603,#339,.T.);
#2054=EDGE_CURVE('',#1603,#1602,#890,.T.);
#2055=EDGE_CURVE('',#1600,#1594,#340,.T.);
#2056=EDGE_CURVE('',#1582,#1592,#1270,.T.);
#2057=EDGE_CURVE('',#1554,#1574,#1271,.T.);
#2058=EDGE_CURVE('',#1591,#1583,#1272,.T.);
#2059=EDGE_CURVE('',#1573,#1555,#1273,.T.);
#2060=EDGE_CURVE('',#1604,#1604,#341,.T.);
#2061=EDGE_CURVE('',#1604,#1605,#891,.T.);
#2062=EDGE_CURVE('',#1605,#1605,#342,.T.);
#2063=EDGE_CURVE('',#1606,#1606,#343,.T.);
#2064=EDGE_CURVE('',#1606,#1607,#344,.T.);
#2065=EDGE_CURVE('',#1607,#1607,#345,.T.);
#2066=EDGE_CURVE('',#1607,#1608,#892,.T.);
#2067=EDGE_CURVE('',#1608,#1608,#346,.T.);
#2068=EDGE_CURVE('',#1608,#1609,#347,.T.);
#2069=EDGE_CURVE('',#1609,#1609,#348,.T.);
#2070=EDGE_CURVE('',#1610,#1610,#349,.T.);
#2071=EDGE_CURVE('',#1610,#1611,#350,.T.);
#2072=EDGE_CURVE('',#1611,#1611,#351,.T.);
#2073=EDGE_CURVE('',#1611,#1612,#893,.T.);
#2074=EDGE_CURVE('',#1612,#1612,#352,.T.);
#2075=EDGE_CURVE('',#1612,#1613,#353,.T.);
#2076=EDGE_CURVE('',#1613,#1613,#354,.T.);
#2077=EDGE_CURVE('',#1614,#1615,#1274,.T.);
#2078=EDGE_CURVE('',#1614,#1616,#894,.T.);
#2079=EDGE_CURVE('',#1617,#1616,#1275,.T.);
#2080=EDGE_CURVE('',#1618,#1617,#895,.T.);
#2081=EDGE_CURVE('',#1619,#1618,#1276,.T.);
#2082=EDGE_CURVE('',#1620,#1619,#896,.T.);
#2083=EDGE_CURVE('',#1621,#1620,#1277,.T.);
#2084=EDGE_CURVE('',#1622,#1621,#897,.T.);
#2085=EDGE_CURVE('',#1623,#1622,#1278,.T.);
#2086=EDGE_CURVE('',#1624,#1623,#898,.T.);
#2087=EDGE_CURVE('',#1625,#1624,#1279,.T.);
#2088=EDGE_CURVE('',#1626,#1625,#899,.T.);
#2089=EDGE_CURVE('',#1627,#1626,#1280,.T.);
#2090=EDGE_CURVE('',#1628,#1627,#900,.T.);
#2091=EDGE_CURVE('',#1629,#1628,#1281,.T.);
#2092=EDGE_CURVE('',#1630,#1629,#901,.T.);
#2093=EDGE_CURVE('',#1631,#1630,#1282,.T.);
#2094=EDGE_CURVE('',#1632,#1631,#902,.T.);
#2095=EDGE_CURVE('',#1633,#1632,#1283,.T.);
#2096=EDGE_CURVE('',#1634,#1633,#903,.T.);
#2097=EDGE_CURVE('',#1635,#1634,#1284,.T.);
#2098=EDGE_CURVE('',#1636,#1635,#904,.T.);
#2099=EDGE_CURVE('',#1637,#1636,#1285,.T.);
#2100=EDGE_CURVE('',#1638,#1637,#905,.T.);
#2101=EDGE_CURVE('',#1639,#1638,#1286,.T.);
#2102=EDGE_CURVE('',#1640,#1639,#906,.T.);
#2103=EDGE_CURVE('',#1641,#1640,#1287,.T.);
#2104=EDGE_CURVE('',#1642,#1641,#907,.T.);
#2105=EDGE_CURVE('',#1643,#1642,#908,.T.);
#2106=EDGE_CURVE('',#1644,#1643,#1288,.T.);
#2107=EDGE_CURVE('',#1645,#1644,#909,.T.);
#2108=EDGE_CURVE('',#1646,#1645,#1289,.T.);
#2109=EDGE_CURVE('',#1647,#1646,#910,.T.);
#2110=EDGE_CURVE('',#1648,#1647,#1290,.T.);
#2111=EDGE_CURVE('',#1649,#1648,#911,.T.);
#2112=EDGE_CURVE('',#1650,#1649,#1291,.T.);
#2113=EDGE_CURVE('',#1651,#1650,#912,.T.);
#2114=EDGE_CURVE('',#1652,#1651,#1292,.T.);
#2115=EDGE_CURVE('',#1653,#1652,#913,.T.);
#2116=EDGE_CURVE('',#1654,#1653,#1293,.T.);
#2117=EDGE_CURVE('',#1655,#1654,#914,.T.);
#2118=EDGE_CURVE('',#1656,#1655,#1294,.T.);
#2119=EDGE_CURVE('',#1657,#1656,#915,.T.);
#2120=EDGE_CURVE('',#1658,#1657,#1295,.T.);
#2121=EDGE_CURVE('',#1659,#1658,#916,.T.);
#2122=EDGE_CURVE('',#1660,#1659,#1296,.T.);
#2123=EDGE_CURVE('',#1661,#1660,#917,.T.);
#2124=EDGE_CURVE('',#1662,#1661,#1297,.T.);
#2125=EDGE_CURVE('',#1663,#1662,#918,.T.);
#2126=EDGE_CURVE('',#1664,#1663,#1298,.T.);
#2127=EDGE_CURVE('',#1665,#1664,#919,.T.);
#2128=EDGE_CURVE('',#1666,#1665,#1299,.T.);
#2129=EDGE_CURVE('',#1667,#1666,#920,.T.);
#2130=EDGE_CURVE('',#1668,#1667,#1300,.T.);
#2131=EDGE_CURVE('',#1615,#1668,#921,.T.);
#2132=EDGE_CURVE('',#1669,#1670,#1301,.T.);
#2133=EDGE_CURVE('',#1671,#1669,#922,.T.);
#2134=EDGE_CURVE('',#1672,#1671,#1302,.T.);
#2135=EDGE_CURVE('',#1673,#1672,#923,.T.);
#2136=EDGE_CURVE('',#1674,#1673,#1303,.T.);
#2137=EDGE_CURVE('',#1675,#1674,#924,.T.);
#2138=EDGE_CURVE('',#1676,#1675,#1304,.T.);
#2139=EDGE_CURVE('',#1677,#1676,#925,.T.);
#2140=EDGE_CURVE('',#1678,#1677,#1305,.T.);
#2141=EDGE_CURVE('',#1679,#1678,#926,.T.);
#2142=EDGE_CURVE('',#1680,#1679,#1306,.T.);
#2143=EDGE_CURVE('',#1681,#1680,#927,.T.);
#2144=EDGE_CURVE('',#1682,#1681,#1307,.T.);
#2145=EDGE_CURVE('',#1683,#1682,#928,.T.);
#2146=EDGE_CURVE('',#1684,#1683,#1308,.T.);
#2147=EDGE_CURVE('',#1685,#1684,#929,.T.);
#2148=EDGE_CURVE('',#1686,#1685,#1309,.T.);
#2149=EDGE_CURVE('',#1687,#1686,#930,.T.);
#2150=EDGE_CURVE('',#1688,#1687,#1310,.T.);
#2151=EDGE_CURVE('',#1689,#1688,#931,.T.);
#2152=EDGE_CURVE('',#1690,#1689,#1311,.T.);
#2153=EDGE_CURVE('',#1691,#1690,#932,.T.);
#2154=EDGE_CURVE('',#1692,#1691,#1312,.T.);
#2155=EDGE_CURVE('',#1693,#1692,#933,.T.);
#2156=EDGE_CURVE('',#1694,#1693,#1313,.T.);
#2157=EDGE_CURVE('',#1695,#1694,#934,.T.);
#2158=EDGE_CURVE('',#1696,#1695,#935,.T.);
#2159=EDGE_CURVE('',#1697,#1696,#1314,.T.);
#2160=EDGE_CURVE('',#1698,#1697,#936,.T.);
#2161=EDGE_CURVE('',#1699,#1698,#1315,.T.);
#2162=EDGE_CURVE('',#1700,#1699,#937,.T.);
#2163=EDGE_CURVE('',#1701,#1700,#1316,.T.);
#2164=EDGE_CURVE('',#1702,#1701,#938,.T.);
#2165=EDGE_CURVE('',#1703,#1702,#1317,.T.);
#2166=EDGE_CURVE('',#1704,#1703,#939,.T.);
#2167=EDGE_CURVE('',#1705,#1704,#1318,.T.);
#2168=EDGE_CURVE('',#1706,#1705,#940,.T.);
#2169=EDGE_CURVE('',#1707,#1706,#1319,.T.);
#2170=EDGE_CURVE('',#1708,#1707,#941,.T.);
#2171=EDGE_CURVE('',#1709,#1708,#1320,.T.);
#2172=EDGE_CURVE('',#1710,#1709,#942,.T.);
#2173=EDGE_CURVE('',#1711,#1710,#1321,.T.);
#2174=EDGE_CURVE('',#1712,#1711,#943,.T.);
#2175=EDGE_CURVE('',#1713,#1712,#1322,.T.);
#2176=EDGE_CURVE('',#1714,#1713,#944,.T.);
#2177=EDGE_CURVE('',#1715,#1714,#1323,.T.);
#2178=EDGE_CURVE('',#1716,#1715,#945,.T.);
#2179=EDGE_CURVE('',#1717,#1716,#1324,.T.);
#2180=EDGE_CURVE('',#1718,#1717,#946,.T.);
#2181=EDGE_CURVE('',#1719,#1718,#1325,.T.);
#2182=EDGE_CURVE('',#1720,#1719,#947,.T.);
#2183=EDGE_CURVE('',#1721,#1720,#1326,.T.);
#2184=EDGE_CURVE('',#1722,#1721,#948,.T.);
#2185=EDGE_CURVE('',#1723,#1722,#1327,.T.);
#2186=EDGE_CURVE('',#1723,#1670,#949,.T.);
#2187=EDGE_CURVE('',#1641,#1724,#1328,.T.);
#2188=EDGE_CURVE('',#1642,#1724,#355,.T.);
#2189=EDGE_CURVE('',#1693,#1644,#1329,.T.);
#2190=EDGE_CURVE('',#1692,#1645,#1330,.T.);
#2191=EDGE_CURVE('',#1637,#1700,#1331,.T.);
#2192=EDGE_CURVE('',#1638,#1699,#1332,.T.);
#2193=EDGE_CURVE('',#1689,#1648,#1333,.T.);
#2194=EDGE_CURVE('',#1688,#1649,#1334,.T.);
#2195=EDGE_CURVE('',#1633,#1704,#1335,.T.);
#2196=EDGE_CURVE('',#1634,#1703,#1336,.T.);
#2197=EDGE_CURVE('',#1685,#1652,#1337,.T.);
#2198=EDGE_CURVE('',#1684,#1653,#1338,.T.);
#2199=EDGE_CURVE('',#1629,#1708,#1339,.T.);
#2200=EDGE_CURVE('',#1630,#1707,#1340,.T.);
#2201=EDGE_CURVE('',#1681,#1656,#1341,.T.);
#2202=EDGE_CURVE('',#1680,#1657,#1342,.T.);
#2203=EDGE_CURVE('',#1625,#1712,#1343,.T.);
#2204=EDGE_CURVE('',#1626,#1711,#1344,.T.);
#2205=EDGE_CURVE('',#1677,#1660,#1345,.T.);
#2206=EDGE_CURVE('',#1676,#1661,#1346,.T.);
#2207=EDGE_CURVE('',#1621,#1716,#1347,.T.);
#2208=EDGE_CURVE('',#1622,#1715,#1348,.T.);
#2209=EDGE_CURVE('',#1673,#1664,#1349,.T.);
#2210=EDGE_CURVE('',#1672,#1665,#1350,.T.);
#2211=EDGE_CURVE('',#1617,#1720,#1351,.T.);
#2212=EDGE_CURVE('',#1618,#1719,#1352,.T.);
#2213=EDGE_CURVE('',#1725,#1668,#1353,.T.);
#2214=EDGE_CURVE('',#1726,#1725,#356,.T.);
#2215=EDGE_CURVE('',#1726,#1615,#1354,.T.);
#2216=EDGE_CURVE('',#1727,#1722,#1355,.T.);
#2217=EDGE_CURVE('',#1723,#1727,#54,.T.);
#2218=EDGE_CURVE('',#1728,#1643,#1356,.T.);
#2219=EDGE_CURVE('',#1694,#1728,#1357,.T.);
#2220=EDGE_CURVE('',#1690,#1647,#1358,.T.);
#2221=EDGE_CURVE('',#1686,#1651,#1359,.T.);
#2222=EDGE_CURVE('',#1682,#1655,#1360,.T.);
#2223=EDGE_CURVE('',#1678,#1659,#1361,.T.);
#2224=EDGE_CURVE('',#1674,#1663,#1362,.T.);
#2225=EDGE_CURVE('',#1669,#1667,#1363,.T.);
#2226=EDGE_CURVE('',#1725,#1670,#55,.T.);
#2227=EDGE_CURVE('',#1639,#1698,#1364,.T.);
#2228=EDGE_CURVE('',#1635,#1702,#1365,.T.);
#2229=EDGE_CURVE('',#1631,#1706,#1366,.T.);
#2230=EDGE_CURVE('',#1627,#1710,#1367,.T.);
#2231=EDGE_CURVE('',#1623,#1714,#1368,.T.);
#2232=EDGE_CURVE('',#1619,#1718,#1369,.T.);
#2233=EDGE_CURVE('',#1724,#1696,#1370,.T.);
#2234=EDGE_CURVE('',#1695,#1728,#357,.F.);
#2235=EDGE_CURVE('',#1721,#1729,#1371,.T.);
#2236=EDGE_CURVE('',#1727,#1729,#358,.T.);
#2237=EDGE_CURVE('',#1697,#1640,#1372,.T.);
#2238=EDGE_CURVE('',#1646,#1691,#1373,.T.);
#2239=EDGE_CURVE('',#1701,#1636,#1374,.T.);
#2240=EDGE_CURVE('',#1650,#1687,#1375,.T.);
#2241=EDGE_CURVE('',#1705,#1632,#1376,.T.);
#2242=EDGE_CURVE('',#1654,#1683,#1377,.T.);
#2243=EDGE_CURVE('',#1709,#1628,#1378,.T.);
#2244=EDGE_CURVE('',#1658,#1679,#1379,.T.);
#2245=EDGE_CURVE('',#1713,#1624,#1380,.T.);
#2246=EDGE_CURVE('',#1662,#1675,#1381,.T.);
#2247=EDGE_CURVE('',#1717,#1620,#1382,.T.);
#2248=EDGE_CURVE('',#1666,#1671,#1383,.T.);
#2249=EDGE_CURVE('',#1729,#1616,#56,.T.);
#2250=EDGE_CURVE('',#1614,#1726,#57,.T.);
#2251=EDGE_CURVE('',#1730,#1730,#359,.T.);
#2252=EDGE_CURVE('',#1730,#1731,#950,.T.);
#2253=EDGE_CURVE('',#1731,#1731,#360,.T.);
#2254=EDGE_CURVE('',#1732,#1732,#361,.T.);
#2255=EDGE_CURVE('',#1732,#1733,#951,.T.);
#2256=EDGE_CURVE('',#1733,#1733,#362,.T.);
#2257=EDGE_CURVE('',#1734,#1734,#363,.T.);
#2258=EDGE_CURVE('',#1733,#1734,#364,.T.);
#2259=EDGE_CURVE('',#1735,#1735,#365,.T.);
#2260=EDGE_CURVE('',#1735,#1736,#366,.T.);
#2261=EDGE_CURVE('',#1736,#1736,#367,.T.);
#2262=EDGE_CURVE('',#1737,#1737,#368,.T.);
#2263=EDGE_CURVE('',#1736,#1737,#952,.T.);
#2264=EDGE_CURVE('',#1738,#1738,#369,.T.);
#2265=EDGE_CURVE('',#1738,#1739,#953,.T.);
#2266=EDGE_CURVE('',#1739,#1739,#370,.T.);
#2267=EDGE_CURVE('',#1740,#1740,#371,.T.);
#2268=EDGE_CURVE('',#1740,#1741,#954,.T.);
#2269=EDGE_CURVE('',#1741,#1741,#372,.T.);
#2270=EDGE_CURVE('',#1742,#1742,#373,.T.);
#2271=EDGE_CURVE('',#1742,#1740,#955,.T.);
#2272=EDGE_CURVE('',#1742,#1743,#956,.T.);
#2273=EDGE_CURVE('',#1743,#1743,#374,.T.);
#2274=EDGE_CURVE('',#1744,#1745,#1384,.T.);
#2275=EDGE_CURVE('',#1745,#1746,#957,.T.);
#2276=EDGE_CURVE('',#1747,#1746,#1385,.T.);
#2277=EDGE_CURVE('',#1744,#1747,#958,.T.);
#2278=EDGE_CURVE('',#1748,#1744,#375,.T.);
#2279=EDGE_CURVE('',#1749,#1747,#376,.T.);
#2280=EDGE_CURVE('',#1748,#1749,#959,.T.);
#2281=EDGE_CURVE('',#1750,#1748,#1386,.T.);
#2282=EDGE_CURVE('',#1751,#1749,#1387,.T.);
#2283=EDGE_CURVE('',#1750,#1751,#960,.T.);
#2284=EDGE_CURVE('',#1745,#1750,#377,.T.);
#2285=EDGE_CURVE('',#1746,#1751,#378,.T.);
#2286=EDGE_CURVE('',#1752,#1753,#961,.T.);
#2287=EDGE_CURVE('',#1753,#1754,#962,.T.);
#2288=EDGE_CURVE('',#1755,#1754,#963,.T.);
#2289=EDGE_CURVE('',#1752,#1755,#964,.T.);
#2290=EDGE_CURVE('',#1756,#1752,#965,.T.);
#2291=EDGE_CURVE('',#1757,#1755,#966,.T.);
#2292=EDGE_CURVE('',#1756,#1757,#967,.T.);
#2293=EDGE_CURVE('',#1758,#1756,#968,.T.);
#2294=EDGE_CURVE('',#1759,#1757,#969,.T.);
#2295=EDGE_CURVE('',#1758,#1759,#970,.T.);
#2296=EDGE_CURVE('',#1760,#1758,#971,.T.);
#2297=EDGE_CURVE('',#1761,#1759,#972,.T.);
#2298=EDGE_CURVE('',#1760,#1761,#973,.T.);
#2299=EDGE_CURVE('',#1762,#1760,#974,.T.);
#2300=EDGE_CURVE('',#1763,#1761,#975,.T.);
#2301=EDGE_CURVE('',#1762,#1763,#976,.T.);
#2302=EDGE_CURVE('',#1753,#1762,#977,.T.);
#2303=EDGE_CURVE('',#1754,#1763,#978,.T.);
#2304=EDGE_CURVE('',#1764,#1765,#1388,.T.);
#2305=EDGE_CURVE('',#1766,#1764,#1389,.T.);
#2306=EDGE_CURVE('',#1767,#1766,#1390,.T.);
#2307=EDGE_CURVE('',#1767,#1765,#1391,.T.);
#2308=EDGE_CURVE('',#1765,#1767,#1392,.T.);
#2309=EDGE_CURVE('',#1764,#1766,#1393,.T.);
#2310=ORIENTED_EDGE('',*,*,#1768,.F.);
#2311=ORIENTED_EDGE('',*,*,#1769,.F.);
#2312=ORIENTED_EDGE('',*,*,#1770,.T.);
#2313=ORIENTED_EDGE('',*,*,#1771,.F.);
#2314=ORIENTED_EDGE('',*,*,#1772,.F.);
#2315=ORIENTED_EDGE('',*,*,#1770,.F.);
#2316=ORIENTED_EDGE('',*,*,#1773,.F.);
#2317=ORIENTED_EDGE('',*,*,#1774,.T.);
#2318=ORIENTED_EDGE('',*,*,#1775,.T.);
#2319=ORIENTED_EDGE('',*,*,#1774,.F.);
#2320=ORIENTED_EDGE('',*,*,#1775,.F.);
#2321=ORIENTED_EDGE('',*,*,#1776,.T.);
#2322=ORIENTED_EDGE('',*,*,#1777,.F.);
#2323=ORIENTED_EDGE('',*,*,#1778,.T.);
#2324=ORIENTED_EDGE('',*,*,#1779,.T.);
#2325=ORIENTED_EDGE('',*,*,#1778,.F.);
#2326=ORIENTED_EDGE('',*,*,#1780,.F.);
#2327=ORIENTED_EDGE('',*,*,#1781,.T.);
#2328=ORIENTED_EDGE('',*,*,#1777,.T.);
#2329=ORIENTED_EDGE('',*,*,#1781,.F.);
#2330=ORIENTED_EDGE('',*,*,#1771,.T.);
#2331=ORIENTED_EDGE('',*,*,#1772,.T.);
#2332=ORIENTED_EDGE('',*,*,#1780,.T.);
#2333=ORIENTED_EDGE('',*,*,#1782,.T.);
#2334=ORIENTED_EDGE('',*,*,#1783,.F.);
#2335=ORIENTED_EDGE('',*,*,#1782,.F.);
#2336=ORIENTED_EDGE('',*,*,#1784,.F.);
#2337=ORIENTED_EDGE('',*,*,#1785,.T.);
#2338=ORIENTED_EDGE('',*,*,#1783,.T.);
#2339=ORIENTED_EDGE('',*,*,#1785,.F.);
#2340=ORIENTED_EDGE('',*,*,#1786,.F.);
#2341=ORIENTED_EDGE('',*,*,#1787,.T.);
#2342=ORIENTED_EDGE('',*,*,#1784,.T.);
#2343=ORIENTED_EDGE('',*,*,#1787,.F.);
#2344=ORIENTED_EDGE('',*,*,#1786,.T.);
#2345=ORIENTED_EDGE('',*,*,#1788,.T.);
#2346=ORIENTED_EDGE('',*,*,#1789,.F.);
#2347=ORIENTED_EDGE('',*,*,#1788,.F.);
#2348=ORIENTED_EDGE('',*,*,#1790,.F.);
#2349=ORIENTED_EDGE('',*,*,#1791,.T.);
#2350=ORIENTED_EDGE('',*,*,#1789,.T.);
#2351=ORIENTED_EDGE('',*,*,#1791,.F.);
#2352=ORIENTED_EDGE('',*,*,#1792,.F.);
#2353=ORIENTED_EDGE('',*,*,#1793,.T.);
#2354=ORIENTED_EDGE('',*,*,#1790,.T.);
#2355=ORIENTED_EDGE('',*,*,#1793,.F.);
#2356=ORIENTED_EDGE('',*,*,#1794,.F.);
#2357=ORIENTED_EDGE('',*,*,#1795,.T.);
#2358=ORIENTED_EDGE('',*,*,#1792,.T.);
#2359=ORIENTED_EDGE('',*,*,#1795,.F.);
#2360=ORIENTED_EDGE('',*,*,#1796,.F.);
#2361=ORIENTED_EDGE('',*,*,#1794,.T.);
#2362=ORIENTED_EDGE('',*,*,#1797,.F.);
#2363=ORIENTED_EDGE('',*,*,#1798,.T.);
#2364=ORIENTED_EDGE('',*,*,#1796,.T.);
#2365=ORIENTED_EDGE('',*,*,#1798,.F.);
#2366=ORIENTED_EDGE('',*,*,#1797,.T.);
#2367=ORIENTED_EDGE('',*,*,#1799,.F.);
#2368=ORIENTED_EDGE('',*,*,#1800,.F.);
#2369=ORIENTED_EDGE('',*,*,#1801,.T.);
#2370=ORIENTED_EDGE('',*,*,#1799,.T.);
#2371=ORIENTED_EDGE('',*,*,#1801,.F.);
#2372=ORIENTED_EDGE('',*,*,#1802,.F.);
#2373=ORIENTED_EDGE('',*,*,#1803,.T.);
#2374=ORIENTED_EDGE('',*,*,#1800,.T.);
#2375=ORIENTED_EDGE('',*,*,#1803,.F.);
#2376=ORIENTED_EDGE('',*,*,#1804,.F.);
#2377=ORIENTED_EDGE('',*,*,#1805,.T.);
#2378=ORIENTED_EDGE('',*,*,#1802,.T.);
#2379=ORIENTED_EDGE('',*,*,#1805,.F.);
#2380=ORIENTED_EDGE('',*,*,#1806,.F.);
#2381=ORIENTED_EDGE('',*,*,#1807,.T.);
#2382=ORIENTED_EDGE('',*,*,#1804,.T.);
#2383=ORIENTED_EDGE('',*,*,#1807,.F.);
#2384=ORIENTED_EDGE('',*,*,#1808,.F.);
#2385=ORIENTED_EDGE('',*,*,#1809,.T.);
#2386=ORIENTED_EDGE('',*,*,#1806,.T.);
#2387=ORIENTED_EDGE('',*,*,#1809,.F.);
#2388=ORIENTED_EDGE('',*,*,#1808,.T.);
#2389=ORIENTED_EDGE('',*,*,#1810,.F.);
#2390=ORIENTED_EDGE('',*,*,#1811,.F.);
#2391=ORIENTED_EDGE('',*,*,#1812,.T.);
#2392=ORIENTED_EDGE('',*,*,#1810,.T.);
#2393=ORIENTED_EDGE('',*,*,#1812,.F.);
#2394=ORIENTED_EDGE('',*,*,#1811,.T.);
#2395=ORIENTED_EDGE('',*,*,#1813,.F.);
#2396=ORIENTED_EDGE('',*,*,#1776,.F.);
#2397=ORIENTED_EDGE('',*,*,#1814,.T.);
#2398=ORIENTED_EDGE('',*,*,#1813,.T.);
#2399=ORIENTED_EDGE('',*,*,#1814,.F.);
#2400=ORIENTED_EDGE('',*,*,#1768,.T.);
#2401=ORIENTED_EDGE('',*,*,#1769,.T.);
#2402=ORIENTED_EDGE('',*,*,#1779,.F.);
#2403=ORIENTED_EDGE('',*,*,#1773,.T.);
#2404=ORIENTED_EDGE('',*,*,#1815,.F.);
#2405=ORIENTED_EDGE('',*,*,#1816,.F.);
#2406=ORIENTED_EDGE('',*,*,#1817,.F.);
#2407=ORIENTED_EDGE('',*,*,#1818,.F.);
#2408=ORIENTED_EDGE('',*,*,#1819,.T.);
#2409=ORIENTED_EDGE('',*,*,#1820,.F.);
#2410=ORIENTED_EDGE('',*,*,#1821,.F.);
#2411=ORIENTED_EDGE('',*,*,#1815,.T.);
#2412=ORIENTED_EDGE('',*,*,#1822,.T.);
#2413=ORIENTED_EDGE('',*,*,#1823,.T.);
#2414=ORIENTED_EDGE('',*,*,#1824,.F.);
#2415=ORIENTED_EDGE('',*,*,#1825,.F.);
#2416=ORIENTED_EDGE('',*,*,#1826,.F.);
#2417=ORIENTED_EDGE('',*,*,#1820,.T.);
#2418=ORIENTED_EDGE('',*,*,#1827,.T.);
#2419=ORIENTED_EDGE('',*,*,#1828,.T.);
#2420=ORIENTED_EDGE('',*,*,#1829,.F.);
#2421=ORIENTED_EDGE('',*,*,#1830,.F.);
#2422=ORIENTED_EDGE('',*,*,#1831,.F.);
#2423=ORIENTED_EDGE('',*,*,#1824,.T.);
#2424=ORIENTED_EDGE('',*,*,#1832,.T.);
#2425=ORIENTED_EDGE('',*,*,#1833,.T.);
#2426=ORIENTED_EDGE('',*,*,#1834,.F.);
#2427=ORIENTED_EDGE('',*,*,#1835,.F.);
#2428=ORIENTED_EDGE('',*,*,#1836,.F.);
#2429=ORIENTED_EDGE('',*,*,#1829,.T.);
#2430=ORIENTED_EDGE('',*,*,#1837,.T.);
#2431=ORIENTED_EDGE('',*,*,#1838,.F.);
#2432=ORIENTED_EDGE('',*,*,#1839,.F.);
#2433=ORIENTED_EDGE('',*,*,#1834,.T.);
#2434=ORIENTED_EDGE('',*,*,#1840,.T.);
#2435=ORIENTED_EDGE('',*,*,#1841,.T.);
#2436=ORIENTED_EDGE('',*,*,#1842,.F.);
#2437=ORIENTED_EDGE('',*,*,#1843,.F.);
#2438=ORIENTED_EDGE('',*,*,#1844,.F.);
#2439=ORIENTED_EDGE('',*,*,#1838,.T.);
#2440=ORIENTED_EDGE('',*,*,#1845,.T.);
#2441=ORIENTED_EDGE('',*,*,#1846,.F.);
#2442=ORIENTED_EDGE('',*,*,#1847,.F.);
#2443=ORIENTED_EDGE('',*,*,#1842,.T.);
#2444=ORIENTED_EDGE('',*,*,#1848,.T.);
#2445=ORIENTED_EDGE('',*,*,#1849,.T.);
#2446=ORIENTED_EDGE('',*,*,#1850,.F.);
#2447=ORIENTED_EDGE('',*,*,#1851,.F.);
#2448=ORIENTED_EDGE('',*,*,#1852,.F.);
#2449=ORIENTED_EDGE('',*,*,#1846,.T.);
#2450=ORIENTED_EDGE('',*,*,#1853,.T.);
#2451=ORIENTED_EDGE('',*,*,#1854,.F.);
#2452=ORIENTED_EDGE('',*,*,#1855,.F.);
#2453=ORIENTED_EDGE('',*,*,#1850,.T.);
#2454=ORIENTED_EDGE('',*,*,#1856,.T.);
#2455=ORIENTED_EDGE('',*,*,#1857,.T.);
#2456=ORIENTED_EDGE('',*,*,#1858,.F.);
#2457=ORIENTED_EDGE('',*,*,#1859,.F.);
#2458=ORIENTED_EDGE('',*,*,#1860,.F.);
#2459=ORIENTED_EDGE('',*,*,#1854,.T.);
#2460=ORIENTED_EDGE('',*,*,#1861,.T.);
#2461=ORIENTED_EDGE('',*,*,#1862,.F.);
#2462=ORIENTED_EDGE('',*,*,#1863,.F.);
#2463=ORIENTED_EDGE('',*,*,#1858,.T.);
#2464=ORIENTED_EDGE('',*,*,#1864,.T.);
#2465=ORIENTED_EDGE('',*,*,#1865,.T.);
#2466=ORIENTED_EDGE('',*,*,#1866,.F.);
#2467=ORIENTED_EDGE('',*,*,#1867,.F.);
#2468=ORIENTED_EDGE('',*,*,#1868,.F.);
#2469=ORIENTED_EDGE('',*,*,#1862,.T.);
#2470=ORIENTED_EDGE('',*,*,#1869,.T.);
#2471=ORIENTED_EDGE('',*,*,#1870,.T.);
#2472=ORIENTED_EDGE('',*,*,#1871,.T.);
#2473=ORIENTED_EDGE('',*,*,#1872,.T.);
#2474=ORIENTED_EDGE('',*,*,#1873,.T.);
#2475=ORIENTED_EDGE('',*,*,#1874,.T.);
#2476=ORIENTED_EDGE('',*,*,#1875,.T.);
#2477=ORIENTED_EDGE('',*,*,#1876,.T.);
#2478=ORIENTED_EDGE('',*,*,#1877,.T.);
#2479=ORIENTED_EDGE('',*,*,#1878,.T.);
#2480=ORIENTED_EDGE('',*,*,#1879,.T.);
#2481=ORIENTED_EDGE('',*,*,#1880,.T.);
#2482=ORIENTED_EDGE('',*,*,#1881,.T.);
#2483=ORIENTED_EDGE('',*,*,#1882,.T.);
#2484=ORIENTED_EDGE('',*,*,#1883,.T.);
#2485=ORIENTED_EDGE('',*,*,#1884,.T.);
#2486=ORIENTED_EDGE('',*,*,#1885,.T.);
#2487=ORIENTED_EDGE('',*,*,#1886,.T.);
#2488=ORIENTED_EDGE('',*,*,#1887,.F.);
#2489=ORIENTED_EDGE('',*,*,#1888,.T.);
#2490=ORIENTED_EDGE('',*,*,#1889,.T.);
#2491=ORIENTED_EDGE('',*,*,#1890,.T.);
#2492=ORIENTED_EDGE('',*,*,#1891,.T.);
#2493=ORIENTED_EDGE('',*,*,#1892,.T.);
#2494=ORIENTED_EDGE('',*,*,#1893,.T.);
#2495=ORIENTED_EDGE('',*,*,#1894,.T.);
#2496=ORIENTED_EDGE('',*,*,#1895,.T.);
#2497=ORIENTED_EDGE('',*,*,#1896,.T.);
#2498=ORIENTED_EDGE('',*,*,#1897,.T.);
#2499=ORIENTED_EDGE('',*,*,#1898,.T.);
#2500=ORIENTED_EDGE('',*,*,#1899,.T.);
#2501=ORIENTED_EDGE('',*,*,#1900,.T.);
#2502=ORIENTED_EDGE('',*,*,#1901,.T.);
#2503=ORIENTED_EDGE('',*,*,#1902,.T.);
#2504=ORIENTED_EDGE('',*,*,#1866,.T.);
#2505=ORIENTED_EDGE('',*,*,#1903,.T.);
#2506=ORIENTED_EDGE('',*,*,#1904,.T.);
#2507=ORIENTED_EDGE('',*,*,#1905,.F.);
#2508=ORIENTED_EDGE('',*,*,#1906,.F.);
#2509=ORIENTED_EDGE('',*,*,#1907,.F.);
#2510=ORIENTED_EDGE('',*,*,#1908,.F.);
#2511=ORIENTED_EDGE('',*,*,#1909,.F.);
#2512=ORIENTED_EDGE('',*,*,#1910,.T.);
#2513=ORIENTED_EDGE('',*,*,#1911,.T.);
#2514=ORIENTED_EDGE('',*,*,#1912,.T.);
#2515=ORIENTED_EDGE('',*,*,#1911,.F.);
#2516=ORIENTED_EDGE('',*,*,#1912,.F.);
#2517=ORIENTED_EDGE('',*,*,#1913,.T.);
#2518=ORIENTED_EDGE('',*,*,#1914,.F.);
#2519=ORIENTED_EDGE('',*,*,#1913,.F.);
#2520=ORIENTED_EDGE('',*,*,#1914,.T.);
#2521=ORIENTED_EDGE('',*,*,#1915,.T.);
#2522=ORIENTED_EDGE('',*,*,#1908,.T.);
#2523=ORIENTED_EDGE('',*,*,#1915,.F.);
#2524=ORIENTED_EDGE('',*,*,#1916,.F.);
#2525=ORIENTED_EDGE('',*,*,#1910,.F.);
#2526=ORIENTED_EDGE('',*,*,#1917,.F.);
#2527=ORIENTED_EDGE('',*,*,#1886,.F.);
#2528=ORIENTED_EDGE('',*,*,#1885,.F.);
#2529=ORIENTED_EDGE('',*,*,#1884,.F.);
#2530=ORIENTED_EDGE('',*,*,#1883,.F.);
#2531=ORIENTED_EDGE('',*,*,#1882,.F.);
#2532=ORIENTED_EDGE('',*,*,#1881,.F.);
#2533=ORIENTED_EDGE('',*,*,#1880,.F.);
#2534=ORIENTED_EDGE('',*,*,#1879,.F.);
#2535=ORIENTED_EDGE('',*,*,#1878,.F.);
#2536=ORIENTED_EDGE('',*,*,#1877,.F.);
#2537=ORIENTED_EDGE('',*,*,#1876,.F.);
#2538=ORIENTED_EDGE('',*,*,#1875,.F.);
#2539=ORIENTED_EDGE('',*,*,#1874,.F.);
#2540=ORIENTED_EDGE('',*,*,#1873,.F.);
#2541=ORIENTED_EDGE('',*,*,#1918,.F.);
#2542=ORIENTED_EDGE('',*,*,#1817,.T.);
#2543=ORIENTED_EDGE('',*,*,#1816,.T.);
#2544=ORIENTED_EDGE('',*,*,#1821,.T.);
#2545=ORIENTED_EDGE('',*,*,#1826,.T.);
#2546=ORIENTED_EDGE('',*,*,#1825,.T.);
#2547=ORIENTED_EDGE('',*,*,#1831,.T.);
#2548=ORIENTED_EDGE('',*,*,#1830,.T.);
#2549=ORIENTED_EDGE('',*,*,#1836,.T.);
#2550=ORIENTED_EDGE('',*,*,#1835,.T.);
#2551=ORIENTED_EDGE('',*,*,#1839,.T.);
#2552=ORIENTED_EDGE('',*,*,#1844,.T.);
#2553=ORIENTED_EDGE('',*,*,#1843,.T.);
#2554=ORIENTED_EDGE('',*,*,#1847,.T.);
#2555=ORIENTED_EDGE('',*,*,#1852,.T.);
#2556=ORIENTED_EDGE('',*,*,#1851,.T.);
#2557=ORIENTED_EDGE('',*,*,#1855,.T.);
#2558=ORIENTED_EDGE('',*,*,#1860,.T.);
#2559=ORIENTED_EDGE('',*,*,#1859,.T.);
#2560=ORIENTED_EDGE('',*,*,#1863,.T.);
#2561=ORIENTED_EDGE('',*,*,#1868,.T.);
#2562=ORIENTED_EDGE('',*,*,#1867,.T.);
#2563=ORIENTED_EDGE('',*,*,#1907,.T.);
#2564=ORIENTED_EDGE('',*,*,#1906,.T.);
#2565=ORIENTED_EDGE('',*,*,#1872,.F.);
#2566=ORIENTED_EDGE('',*,*,#1919,.T.);
#2567=ORIENTED_EDGE('',*,*,#1818,.T.);
#2568=ORIENTED_EDGE('',*,*,#1918,.T.);
#2569=ORIENTED_EDGE('',*,*,#1920,.F.);
#2570=ORIENTED_EDGE('',*,*,#1904,.F.);
#2571=ORIENTED_EDGE('',*,*,#1903,.F.);
#2572=ORIENTED_EDGE('',*,*,#1870,.F.);
#2573=ORIENTED_EDGE('',*,*,#1869,.F.);
#2574=ORIENTED_EDGE('',*,*,#1865,.F.);
#2575=ORIENTED_EDGE('',*,*,#1864,.F.);
#2576=ORIENTED_EDGE('',*,*,#1861,.F.);
#2577=ORIENTED_EDGE('',*,*,#1857,.F.);
#2578=ORIENTED_EDGE('',*,*,#1856,.F.);
#2579=ORIENTED_EDGE('',*,*,#1853,.F.);
#2580=ORIENTED_EDGE('',*,*,#1849,.F.);
#2581=ORIENTED_EDGE('',*,*,#1848,.F.);
#2582=ORIENTED_EDGE('',*,*,#1845,.F.);
#2583=ORIENTED_EDGE('',*,*,#1841,.F.);
#2584=ORIENTED_EDGE('',*,*,#1840,.F.);
#2585=ORIENTED_EDGE('',*,*,#1837,.F.);
#2586=ORIENTED_EDGE('',*,*,#1833,.F.);
#2587=ORIENTED_EDGE('',*,*,#1832,.F.);
#2588=ORIENTED_EDGE('',*,*,#1828,.F.);
#2589=ORIENTED_EDGE('',*,*,#1827,.F.);
#2590=ORIENTED_EDGE('',*,*,#1823,.F.);
#2591=ORIENTED_EDGE('',*,*,#1822,.F.);
#2592=ORIENTED_EDGE('',*,*,#1819,.F.);
#2593=ORIENTED_EDGE('',*,*,#1919,.F.);
#2594=ORIENTED_EDGE('',*,*,#1902,.F.);
#2595=ORIENTED_EDGE('',*,*,#1901,.F.);
#2596=ORIENTED_EDGE('',*,*,#1900,.F.);
#2597=ORIENTED_EDGE('',*,*,#1899,.F.);
#2598=ORIENTED_EDGE('',*,*,#1898,.F.);
#2599=ORIENTED_EDGE('',*,*,#1897,.F.);
#2600=ORIENTED_EDGE('',*,*,#1896,.F.);
#2601=ORIENTED_EDGE('',*,*,#1895,.F.);
#2602=ORIENTED_EDGE('',*,*,#1894,.F.);
#2603=ORIENTED_EDGE('',*,*,#1893,.F.);
#2604=ORIENTED_EDGE('',*,*,#1892,.F.);
#2605=ORIENTED_EDGE('',*,*,#1891,.F.);
#2606=ORIENTED_EDGE('',*,*,#1890,.F.);
#2607=ORIENTED_EDGE('',*,*,#1889,.F.);
#2608=ORIENTED_EDGE('',*,*,#1888,.F.);
#2609=ORIENTED_EDGE('',*,*,#1917,.T.);
#2610=ORIENTED_EDGE('',*,*,#1905,.T.);
#2611=ORIENTED_EDGE('',*,*,#1920,.T.);
#2612=ORIENTED_EDGE('',*,*,#1887,.T.);
#2613=ORIENTED_EDGE('',*,*,#1921,.T.);
#2614=ORIENTED_EDGE('',*,*,#1922,.T.);
#2615=ORIENTED_EDGE('',*,*,#1923,.T.);
#2616=ORIENTED_EDGE('',*,*,#1922,.F.);
#2617=ORIENTED_EDGE('',*,*,#1923,.F.);
#2618=ORIENTED_EDGE('',*,*,#1924,.T.);
#2619=ORIENTED_EDGE('',*,*,#1925,.T.);
#2620=ORIENTED_EDGE('',*,*,#1924,.F.);
#2621=ORIENTED_EDGE('',*,*,#1921,.F.);
#2622=ORIENTED_EDGE('',*,*,#1871,.F.);
#2623=ORIENTED_EDGE('',*,*,#1926,.T.);
#2624=ORIENTED_EDGE('',*,*,#1927,.T.);
#2625=ORIENTED_EDGE('',*,*,#1928,.T.);
#2626=ORIENTED_EDGE('',*,*,#1927,.F.);
#2627=ORIENTED_EDGE('',*,*,#1928,.F.);
#2628=ORIENTED_EDGE('',*,*,#1929,.T.);
#2629=ORIENTED_EDGE('',*,*,#1930,.F.);
#2630=ORIENTED_EDGE('',*,*,#1929,.F.);
#2631=ORIENTED_EDGE('',*,*,#1926,.F.);
#2632=ORIENTED_EDGE('',*,*,#1925,.F.);
#2633=ORIENTED_EDGE('',*,*,#1930,.T.);
#2634=ORIENTED_EDGE('',*,*,#1931,.T.);
#2635=ORIENTED_EDGE('',*,*,#1932,.T.);
#2636=ORIENTED_EDGE('',*,*,#1931,.F.);
#2637=ORIENTED_EDGE('',*,*,#1932,.F.);
#2638=ORIENTED_EDGE('',*,*,#1933,.T.);
#2639=ORIENTED_EDGE('',*,*,#1934,.T.);
#2640=ORIENTED_EDGE('',*,*,#1935,.T.);
#2641=ORIENTED_EDGE('',*,*,#1936,.T.);
#2642=ORIENTED_EDGE('',*,*,#1935,.F.);
#2643=ORIENTED_EDGE('',*,*,#1936,.F.);
#2644=ORIENTED_EDGE('',*,*,#1937,.T.);
#2645=ORIENTED_EDGE('',*,*,#1938,.F.);
#2646=ORIENTED_EDGE('',*,*,#1937,.F.);
#2647=ORIENTED_EDGE('',*,*,#1934,.F.);
#2648=ORIENTED_EDGE('',*,*,#1939,.F.);
#2649=ORIENTED_EDGE('',*,*,#1938,.T.);
#2650=ORIENTED_EDGE('',*,*,#1940,.T.);
#2651=ORIENTED_EDGE('',*,*,#1916,.T.);
#2652=ORIENTED_EDGE('',*,*,#1940,.F.);
#2653=ORIENTED_EDGE('',*,*,#1909,.T.);
#2654=ORIENTED_EDGE('',*,*,#1941,.T.);
#2655=ORIENTED_EDGE('',*,*,#1942,.T.);
#2656=ORIENTED_EDGE('',*,*,#1941,.F.);
#2657=ORIENTED_EDGE('',*,*,#1942,.F.);
#2658=ORIENTED_EDGE('',*,*,#1943,.T.);
#2659=ORIENTED_EDGE('',*,*,#1944,.F.);
#2660=ORIENTED_EDGE('',*,*,#1943,.F.);
#2661=ORIENTED_EDGE('',*,*,#1944,.T.);
#2662=ORIENTED_EDGE('',*,*,#1945,.T.);
#2663=ORIENTED_EDGE('',*,*,#1946,.T.);
#2664=ORIENTED_EDGE('',*,*,#1945,.F.);
#2665=ORIENTED_EDGE('',*,*,#1946,.F.);
#2666=ORIENTED_EDGE('',*,*,#1947,.T.);
#2667=ORIENTED_EDGE('',*,*,#1948,.T.);
#2668=ORIENTED_EDGE('',*,*,#1949,.T.);
#2669=ORIENTED_EDGE('',*,*,#1950,.T.);
#2670=ORIENTED_EDGE('',*,*,#1949,.F.);
#2671=ORIENTED_EDGE('',*,*,#1950,.F.);
#2672=ORIENTED_EDGE('',*,*,#1951,.T.);
#2673=ORIENTED_EDGE('',*,*,#1952,.F.);
#2674=ORIENTED_EDGE('',*,*,#1951,.F.);
#2675=ORIENTED_EDGE('',*,*,#1948,.F.);
#2676=ORIENTED_EDGE('',*,*,#1953,.F.);
#2677=ORIENTED_EDGE('',*,*,#1952,.T.);
#2678=ORIENTED_EDGE('',*,*,#1954,.T.);
#2679=ORIENTED_EDGE('',*,*,#1955,.T.);
#2680=ORIENTED_EDGE('',*,*,#1954,.F.);
#2681=ORIENTED_EDGE('',*,*,#1955,.F.);
#2682=ORIENTED_EDGE('',*,*,#1956,.T.);
#2683=ORIENTED_EDGE('',*,*,#1957,.T.);
#2684=ORIENTED_EDGE('',*,*,#1958,.T.);
#2685=ORIENTED_EDGE('',*,*,#1959,.T.);
#2686=ORIENTED_EDGE('',*,*,#1958,.F.);
#2687=ORIENTED_EDGE('',*,*,#1959,.F.);
#2688=ORIENTED_EDGE('',*,*,#1956,.F.);
#2689=ORIENTED_EDGE('',*,*,#1960,.T.);
#2690=ORIENTED_EDGE('',*,*,#1957,.F.);
#2691=ORIENTED_EDGE('',*,*,#1960,.F.);
#2692=ORIENTED_EDGE('',*,*,#1947,.F.);
#2693=ORIENTED_EDGE('',*,*,#1961,.T.);
#2694=ORIENTED_EDGE('',*,*,#1953,.T.);
#2695=ORIENTED_EDGE('',*,*,#1961,.F.);
#2696=ORIENTED_EDGE('',*,*,#1933,.F.);
#2697=ORIENTED_EDGE('',*,*,#1962,.T.);
#2698=ORIENTED_EDGE('',*,*,#1939,.T.);
#2699=ORIENTED_EDGE('',*,*,#1962,.F.);
#2700=ORIENTED_EDGE('',*,*,#1963,.T.);
#2701=ORIENTED_EDGE('',*,*,#1964,.T.);
#2702=ORIENTED_EDGE('',*,*,#1965,.F.);
#2703=ORIENTED_EDGE('',*,*,#1966,.F.);
#2704=ORIENTED_EDGE('',*,*,#1967,.T.);
#2705=ORIENTED_EDGE('',*,*,#1966,.T.);
#2706=ORIENTED_EDGE('',*,*,#1968,.F.);
#2707=ORIENTED_EDGE('',*,*,#1969,.F.);
#2708=ORIENTED_EDGE('',*,*,#1970,.T.);
#2709=ORIENTED_EDGE('',*,*,#1969,.T.);
#2710=ORIENTED_EDGE('',*,*,#1971,.F.);
#2711=ORIENTED_EDGE('',*,*,#1972,.F.);
#2712=ORIENTED_EDGE('',*,*,#1973,.T.);
#2713=ORIENTED_EDGE('',*,*,#1972,.T.);
#2714=ORIENTED_EDGE('',*,*,#1974,.F.);
#2715=ORIENTED_EDGE('',*,*,#1964,.F.);
#2716=ORIENTED_EDGE('',*,*,#1975,.T.);
#2717=ORIENTED_EDGE('',*,*,#1976,.T.);
#2718=ORIENTED_EDGE('',*,*,#1977,.F.);
#2719=ORIENTED_EDGE('',*,*,#1978,.F.);
#2720=ORIENTED_EDGE('',*,*,#1979,.T.);
#2721=ORIENTED_EDGE('',*,*,#1978,.T.);
#2722=ORIENTED_EDGE('',*,*,#1980,.F.);
#2723=ORIENTED_EDGE('',*,*,#1981,.F.);
#2724=ORIENTED_EDGE('',*,*,#1982,.T.);
#2725=ORIENTED_EDGE('',*,*,#1981,.T.);
#2726=ORIENTED_EDGE('',*,*,#1983,.F.);
#2727=ORIENTED_EDGE('',*,*,#1984,.F.);
#2728=ORIENTED_EDGE('',*,*,#1985,.T.);
#2729=ORIENTED_EDGE('',*,*,#1984,.T.);
#2730=ORIENTED_EDGE('',*,*,#1986,.F.);
#2731=ORIENTED_EDGE('',*,*,#1987,.F.);
#2732=ORIENTED_EDGE('',*,*,#1988,.T.);
#2733=ORIENTED_EDGE('',*,*,#1987,.T.);
#2734=ORIENTED_EDGE('',*,*,#1989,.F.);
#2735=ORIENTED_EDGE('',*,*,#1990,.F.);
#2736=ORIENTED_EDGE('',*,*,#1991,.T.);
#2737=ORIENTED_EDGE('',*,*,#1990,.T.);
#2738=ORIENTED_EDGE('',*,*,#1992,.F.);
#2739=ORIENTED_EDGE('',*,*,#1976,.F.);
#2740=ORIENTED_EDGE('',*,*,#1992,.T.);
#2741=ORIENTED_EDGE('',*,*,#1989,.T.);
#2742=ORIENTED_EDGE('',*,*,#1986,.T.);
#2743=ORIENTED_EDGE('',*,*,#1983,.T.);
#2744=ORIENTED_EDGE('',*,*,#1980,.T.);
#2745=ORIENTED_EDGE('',*,*,#1977,.T.);
#2746=ORIENTED_EDGE('',*,*,#1974,.T.);
#2747=ORIENTED_EDGE('',*,*,#1971,.T.);
#2748=ORIENTED_EDGE('',*,*,#1968,.T.);
#2749=ORIENTED_EDGE('',*,*,#1965,.T.);
#2750=ORIENTED_EDGE('',*,*,#1991,.F.);
#2751=ORIENTED_EDGE('',*,*,#1975,.F.);
#2752=ORIENTED_EDGE('',*,*,#1979,.F.);
#2753=ORIENTED_EDGE('',*,*,#1982,.F.);
#2754=ORIENTED_EDGE('',*,*,#1985,.F.);
#2755=ORIENTED_EDGE('',*,*,#1988,.F.);
#2756=ORIENTED_EDGE('',*,*,#1973,.F.);
#2757=ORIENTED_EDGE('',*,*,#1963,.F.);
#2758=ORIENTED_EDGE('',*,*,#1967,.F.);
#2759=ORIENTED_EDGE('',*,*,#1970,.F.);
#2760=ORIENTED_EDGE('',*,*,#1993,.F.);
#2761=ORIENTED_EDGE('',*,*,#1994,.F.);
#2762=ORIENTED_EDGE('',*,*,#1995,.F.);
#2763=ORIENTED_EDGE('',*,*,#1996,.T.);
#2764=ORIENTED_EDGE('',*,*,#1997,.F.);
#2765=ORIENTED_EDGE('',*,*,#1998,.F.);
#2766=ORIENTED_EDGE('',*,*,#1999,.F.);
#2767=ORIENTED_EDGE('',*,*,#1993,.T.);
#2768=ORIENTED_EDGE('',*,*,#2000,.T.);
#2769=ORIENTED_EDGE('',*,*,#2001,.T.);
#2770=ORIENTED_EDGE('',*,*,#2002,.F.);
#2771=ORIENTED_EDGE('',*,*,#2003,.F.);
#2772=ORIENTED_EDGE('',*,*,#2004,.F.);
#2773=ORIENTED_EDGE('',*,*,#1997,.T.);
#2774=ORIENTED_EDGE('',*,*,#2005,.T.);
#2775=ORIENTED_EDGE('',*,*,#2006,.F.);
#2776=ORIENTED_EDGE('',*,*,#2007,.F.);
#2777=ORIENTED_EDGE('',*,*,#2002,.T.);
#2778=ORIENTED_EDGE('',*,*,#2008,.T.);
#2779=ORIENTED_EDGE('',*,*,#2009,.T.);
#2780=ORIENTED_EDGE('',*,*,#2010,.F.);
#2781=ORIENTED_EDGE('',*,*,#2011,.F.);
#2782=ORIENTED_EDGE('',*,*,#2012,.F.);
#2783=ORIENTED_EDGE('',*,*,#2006,.T.);
#2784=ORIENTED_EDGE('',*,*,#2013,.T.);
#2785=ORIENTED_EDGE('',*,*,#2014,.F.);
#2786=ORIENTED_EDGE('',*,*,#2015,.F.);
#2787=ORIENTED_EDGE('',*,*,#2010,.T.);
#2788=ORIENTED_EDGE('',*,*,#2016,.T.);
#2789=ORIENTED_EDGE('',*,*,#2017,.T.);
#2790=ORIENTED_EDGE('',*,*,#2018,.T.);
#2791=ORIENTED_EDGE('',*,*,#2019,.T.);
#2792=ORIENTED_EDGE('',*,*,#2020,.T.);
#2793=ORIENTED_EDGE('',*,*,#2021,.T.);
#2794=ORIENTED_EDGE('',*,*,#2022,.T.);
#2795=ORIENTED_EDGE('',*,*,#2023,.T.);
#2796=ORIENTED_EDGE('',*,*,#2024,.T.);
#2797=ORIENTED_EDGE('',*,*,#2025,.T.);
#2798=ORIENTED_EDGE('',*,*,#2026,.T.);
#2799=ORIENTED_EDGE('',*,*,#2027,.T.);
#2800=ORIENTED_EDGE('',*,*,#2028,.F.);
#2801=ORIENTED_EDGE('',*,*,#2029,.T.);
#2802=ORIENTED_EDGE('',*,*,#2030,.T.);
#2803=ORIENTED_EDGE('',*,*,#2031,.T.);
#2804=ORIENTED_EDGE('',*,*,#2032,.T.);
#2805=ORIENTED_EDGE('',*,*,#2033,.T.);
#2806=ORIENTED_EDGE('',*,*,#2034,.T.);
#2807=ORIENTED_EDGE('',*,*,#2035,.T.);
#2808=ORIENTED_EDGE('',*,*,#2014,.T.);
#2809=ORIENTED_EDGE('',*,*,#2036,.T.);
#2810=ORIENTED_EDGE('',*,*,#2037,.T.);
#2811=ORIENTED_EDGE('',*,*,#2038,.F.);
#2812=ORIENTED_EDGE('',*,*,#2039,.F.);
#2813=ORIENTED_EDGE('',*,*,#2040,.F.);
#2814=ORIENTED_EDGE('',*,*,#2041,.F.);
#2815=ORIENTED_EDGE('',*,*,#2042,.T.);
#2816=ORIENTED_EDGE('',*,*,#2043,.T.);
#2817=ORIENTED_EDGE('',*,*,#2044,.T.);
#2818=ORIENTED_EDGE('',*,*,#2045,.F.);
#2819=ORIENTED_EDGE('',*,*,#2044,.F.);
#2820=ORIENTED_EDGE('',*,*,#2046,.T.);
#2821=ORIENTED_EDGE('',*,*,#2047,.T.);
#2822=ORIENTED_EDGE('',*,*,#2048,.F.);
#2823=ORIENTED_EDGE('',*,*,#2047,.F.);
#2824=ORIENTED_EDGE('',*,*,#2049,.T.);
#2825=ORIENTED_EDGE('',*,*,#2050,.T.);
#2826=ORIENTED_EDGE('',*,*,#2051,.T.);
#2827=ORIENTED_EDGE('',*,*,#2052,.T.);
#2828=ORIENTED_EDGE('',*,*,#2049,.F.);
#2829=ORIENTED_EDGE('',*,*,#2046,.F.);
#2830=ORIENTED_EDGE('',*,*,#2043,.F.);
#2831=ORIENTED_EDGE('',*,*,#2053,.F.);
#2832=ORIENTED_EDGE('',*,*,#2054,.T.);
#2833=ORIENTED_EDGE('',*,*,#2051,.F.);
#2834=ORIENTED_EDGE('',*,*,#2042,.F.);
#2835=ORIENTED_EDGE('',*,*,#2055,.F.);
#2836=ORIENTED_EDGE('',*,*,#2050,.F.);
#2837=ORIENTED_EDGE('',*,*,#2052,.F.);
#2838=ORIENTED_EDGE('',*,*,#2054,.F.);
#2839=ORIENTED_EDGE('',*,*,#2056,.F.);
#2840=ORIENTED_EDGE('',*,*,#2027,.F.);
#2841=ORIENTED_EDGE('',*,*,#2026,.F.);
#2842=ORIENTED_EDGE('',*,*,#2025,.F.);
#2843=ORIENTED_EDGE('',*,*,#2024,.F.);
#2844=ORIENTED_EDGE('',*,*,#2023,.F.);
#2845=ORIENTED_EDGE('',*,*,#2022,.F.);
#2846=ORIENTED_EDGE('',*,*,#2021,.F.);
#2847=ORIENTED_EDGE('',*,*,#2020,.F.);
#2848=ORIENTED_EDGE('',*,*,#2057,.F.);
#2849=ORIENTED_EDGE('',*,*,#1994,.T.);
#2850=ORIENTED_EDGE('',*,*,#1999,.T.);
#2851=ORIENTED_EDGE('',*,*,#1998,.T.);
#2852=ORIENTED_EDGE('',*,*,#2004,.T.);
#2853=ORIENTED_EDGE('',*,*,#2003,.T.);
#2854=ORIENTED_EDGE('',*,*,#2007,.T.);
#2855=ORIENTED_EDGE('',*,*,#2012,.T.);
#2856=ORIENTED_EDGE('',*,*,#2011,.T.);
#2857=ORIENTED_EDGE('',*,*,#2015,.T.);
#2858=ORIENTED_EDGE('',*,*,#2040,.T.);
#2859=ORIENTED_EDGE('',*,*,#2039,.T.);
#2860=ORIENTED_EDGE('',*,*,#2058,.F.);
#2861=ORIENTED_EDGE('',*,*,#2037,.F.);
#2862=ORIENTED_EDGE('',*,*,#2036,.F.);
#2863=ORIENTED_EDGE('',*,*,#2017,.F.);
#2864=ORIENTED_EDGE('',*,*,#2016,.F.);
#2865=ORIENTED_EDGE('',*,*,#2013,.F.);
#2866=ORIENTED_EDGE('',*,*,#2009,.F.);
#2867=ORIENTED_EDGE('',*,*,#2008,.F.);
#2868=ORIENTED_EDGE('',*,*,#2005,.F.);
#2869=ORIENTED_EDGE('',*,*,#2001,.F.);
#2870=ORIENTED_EDGE('',*,*,#2000,.F.);
#2871=ORIENTED_EDGE('',*,*,#1996,.F.);
#2872=ORIENTED_EDGE('',*,*,#2059,.F.);
#2873=ORIENTED_EDGE('',*,*,#2018,.F.);
#2874=ORIENTED_EDGE('',*,*,#2035,.F.);
#2875=ORIENTED_EDGE('',*,*,#2034,.F.);
#2876=ORIENTED_EDGE('',*,*,#2033,.F.);
#2877=ORIENTED_EDGE('',*,*,#2032,.F.);
#2878=ORIENTED_EDGE('',*,*,#2031,.F.);
#2879=ORIENTED_EDGE('',*,*,#2030,.F.);
#2880=ORIENTED_EDGE('',*,*,#2029,.F.);
#2881=ORIENTED_EDGE('',*,*,#2060,.F.);
#2882=ORIENTED_EDGE('',*,*,#2061,.T.);
#2883=ORIENTED_EDGE('',*,*,#2062,.T.);
#2884=ORIENTED_EDGE('',*,*,#2061,.F.);
#2885=ORIENTED_EDGE('',*,*,#2060,.T.);
#2886=ORIENTED_EDGE('',*,*,#2059,.T.);
#2887=ORIENTED_EDGE('',*,*,#1995,.T.);
#2888=ORIENTED_EDGE('',*,*,#2057,.T.);
#2889=ORIENTED_EDGE('',*,*,#2019,.F.);
#2890=ORIENTED_EDGE('',*,*,#2058,.T.);
#2891=ORIENTED_EDGE('',*,*,#2028,.T.);
#2892=ORIENTED_EDGE('',*,*,#2056,.T.);
#2893=ORIENTED_EDGE('',*,*,#2038,.T.);
#2894=ORIENTED_EDGE('',*,*,#2048,.T.);
#2895=ORIENTED_EDGE('',*,*,#2055,.T.);
#2896=ORIENTED_EDGE('',*,*,#2041,.T.);
#2897=ORIENTED_EDGE('',*,*,#2045,.T.);
#2898=ORIENTED_EDGE('',*,*,#2062,.F.);
#2899=ORIENTED_EDGE('',*,*,#2053,.T.);
#2900=ORIENTED_EDGE('',*,*,#2063,.T.);
#2901=ORIENTED_EDGE('',*,*,#2064,.T.);
#2902=ORIENTED_EDGE('',*,*,#2065,.T.);
#2903=ORIENTED_EDGE('',*,*,#2064,.F.);
#2904=ORIENTED_EDGE('',*,*,#2065,.F.);
#2905=ORIENTED_EDGE('',*,*,#2066,.T.);
#2906=ORIENTED_EDGE('',*,*,#2067,.F.);
#2907=ORIENTED_EDGE('',*,*,#2066,.F.);
#2908=ORIENTED_EDGE('',*,*,#2063,.F.);
#2909=ORIENTED_EDGE('',*,*,#2067,.T.);
#2910=ORIENTED_EDGE('',*,*,#2068,.T.);
#2911=ORIENTED_EDGE('',*,*,#2069,.T.);
#2912=ORIENTED_EDGE('',*,*,#2068,.F.);
#2913=ORIENTED_EDGE('',*,*,#2069,.F.);
#2914=ORIENTED_EDGE('',*,*,#2070,.T.);
#2915=ORIENTED_EDGE('',*,*,#2071,.T.);
#2916=ORIENTED_EDGE('',*,*,#2072,.T.);
#2917=ORIENTED_EDGE('',*,*,#2071,.F.);
#2918=ORIENTED_EDGE('',*,*,#2072,.F.);
#2919=ORIENTED_EDGE('',*,*,#2073,.T.);
#2920=ORIENTED_EDGE('',*,*,#2074,.F.);
#2921=ORIENTED_EDGE('',*,*,#2073,.F.);
#2922=ORIENTED_EDGE('',*,*,#2070,.F.);
#2923=ORIENTED_EDGE('',*,*,#2074,.T.);
#2924=ORIENTED_EDGE('',*,*,#2075,.T.);
#2925=ORIENTED_EDGE('',*,*,#2076,.T.);
#2926=ORIENTED_EDGE('',*,*,#2075,.F.);
#2927=ORIENTED_EDGE('',*,*,#2076,.F.);
#2928=ORIENTED_EDGE('',*,*,#2077,.F.);
#2929=ORIENTED_EDGE('',*,*,#2078,.T.);
#2930=ORIENTED_EDGE('',*,*,#2079,.F.);
#2931=ORIENTED_EDGE('',*,*,#2080,.F.);
#2932=ORIENTED_EDGE('',*,*,#2081,.F.);
#2933=ORIENTED_EDGE('',*,*,#2082,.F.);
#2934=ORIENTED_EDGE('',*,*,#2083,.F.);
#2935=ORIENTED_EDGE('',*,*,#2084,.F.);
#2936=ORIENTED_EDGE('',*,*,#2085,.F.);
#2937=ORIENTED_EDGE('',*,*,#2086,.F.);
#2938=ORIENTED_EDGE('',*,*,#2087,.F.);
#2939=ORIENTED_EDGE('',*,*,#2088,.F.);
#2940=ORIENTED_EDGE('',*,*,#2089,.F.);
#2941=ORIENTED_EDGE('',*,*,#2090,.F.);
#2942=ORIENTED_EDGE('',*,*,#2091,.F.);
#2943=ORIENTED_EDGE('',*,*,#2092,.F.);
#2944=ORIENTED_EDGE('',*,*,#2093,.F.);
#2945=ORIENTED_EDGE('',*,*,#2094,.F.);
#2946=ORIENTED_EDGE('',*,*,#2095,.F.);
#2947=ORIENTED_EDGE('',*,*,#2096,.F.);
#2948=ORIENTED_EDGE('',*,*,#2097,.F.);
#2949=ORIENTED_EDGE('',*,*,#2098,.F.);
#2950=ORIENTED_EDGE('',*,*,#2099,.F.);
#2951=ORIENTED_EDGE('',*,*,#2100,.F.);
#2952=ORIENTED_EDGE('',*,*,#2101,.F.);
#2953=ORIENTED_EDGE('',*,*,#2102,.F.);
#2954=ORIENTED_EDGE('',*,*,#2103,.F.);
#2955=ORIENTED_EDGE('',*,*,#2104,.F.);
#2956=ORIENTED_EDGE('',*,*,#2105,.F.);
#2957=ORIENTED_EDGE('',*,*,#2106,.F.);
#2958=ORIENTED_EDGE('',*,*,#2107,.F.);
#2959=ORIENTED_EDGE('',*,*,#2108,.F.);
#2960=ORIENTED_EDGE('',*,*,#2109,.F.);
#2961=ORIENTED_EDGE('',*,*,#2110,.F.);
#2962=ORIENTED_EDGE('',*,*,#2111,.F.);
#2963=ORIENTED_EDGE('',*,*,#2112,.F.);
#2964=ORIENTED_EDGE('',*,*,#2113,.F.);
#2965=ORIENTED_EDGE('',*,*,#2114,.F.);
#2966=ORIENTED_EDGE('',*,*,#2115,.F.);
#2967=ORIENTED_EDGE('',*,*,#2116,.F.);
#2968=ORIENTED_EDGE('',*,*,#2117,.F.);
#2969=ORIENTED_EDGE('',*,*,#2118,.F.);
#2970=ORIENTED_EDGE('',*,*,#2119,.F.);
#2971=ORIENTED_EDGE('',*,*,#2120,.F.);
#2972=ORIENTED_EDGE('',*,*,#2121,.F.);
#2973=ORIENTED_EDGE('',*,*,#2122,.F.);
#2974=ORIENTED_EDGE('',*,*,#2123,.F.);
#2975=ORIENTED_EDGE('',*,*,#2124,.F.);
#2976=ORIENTED_EDGE('',*,*,#2125,.F.);
#2977=ORIENTED_EDGE('',*,*,#2126,.F.);
#2978=ORIENTED_EDGE('',*,*,#2127,.F.);
#2979=ORIENTED_EDGE('',*,*,#2128,.F.);
#2980=ORIENTED_EDGE('',*,*,#2129,.F.);
#2981=ORIENTED_EDGE('',*,*,#2130,.F.);
#2982=ORIENTED_EDGE('',*,*,#2131,.F.);
#2983=ORIENTED_EDGE('',*,*,#2132,.F.);
#2984=ORIENTED_EDGE('',*,*,#2133,.F.);
#2985=ORIENTED_EDGE('',*,*,#2134,.F.);
#2986=ORIENTED_EDGE('',*,*,#2135,.F.);
#2987=ORIENTED_EDGE('',*,*,#2136,.F.);
#2988=ORIENTED_EDGE('',*,*,#2137,.F.);
#2989=ORIENTED_EDGE('',*,*,#2138,.F.);
#2990=ORIENTED_EDGE('',*,*,#2139,.F.);
#2991=ORIENTED_EDGE('',*,*,#2140,.F.);
#2992=ORIENTED_EDGE('',*,*,#2141,.F.);
#2993=ORIENTED_EDGE('',*,*,#2142,.F.);
#2994=ORIENTED_EDGE('',*,*,#2143,.F.);
#2995=ORIENTED_EDGE('',*,*,#2144,.F.);
#2996=ORIENTED_EDGE('',*,*,#2145,.F.);
#2997=ORIENTED_EDGE('',*,*,#2146,.F.);
#2998=ORIENTED_EDGE('',*,*,#2147,.F.);
#2999=ORIENTED_EDGE('',*,*,#2148,.F.);
#3000=ORIENTED_EDGE('',*,*,#2149,.F.);
#3001=ORIENTED_EDGE('',*,*,#2150,.F.);
#3002=ORIENTED_EDGE('',*,*,#2151,.F.);
#3003=ORIENTED_EDGE('',*,*,#2152,.F.);
#3004=ORIENTED_EDGE('',*,*,#2153,.F.);
#3005=ORIENTED_EDGE('',*,*,#2154,.F.);
#3006=ORIENTED_EDGE('',*,*,#2155,.F.);
#3007=ORIENTED_EDGE('',*,*,#2156,.F.);
#3008=ORIENTED_EDGE('',*,*,#2157,.F.);
#3009=ORIENTED_EDGE('',*,*,#2158,.F.);
#3010=ORIENTED_EDGE('',*,*,#2159,.F.);
#3011=ORIENTED_EDGE('',*,*,#2160,.F.);
#3012=ORIENTED_EDGE('',*,*,#2161,.F.);
#3013=ORIENTED_EDGE('',*,*,#2162,.F.);
#3014=ORIENTED_EDGE('',*,*,#2163,.F.);
#3015=ORIENTED_EDGE('',*,*,#2164,.F.);
#3016=ORIENTED_EDGE('',*,*,#2165,.F.);
#3017=ORIENTED_EDGE('',*,*,#2166,.F.);
#3018=ORIENTED_EDGE('',*,*,#2167,.F.);
#3019=ORIENTED_EDGE('',*,*,#2168,.F.);
#3020=ORIENTED_EDGE('',*,*,#2169,.F.);
#3021=ORIENTED_EDGE('',*,*,#2170,.F.);
#3022=ORIENTED_EDGE('',*,*,#2171,.F.);
#3023=ORIENTED_EDGE('',*,*,#2172,.F.);
#3024=ORIENTED_EDGE('',*,*,#2173,.F.);
#3025=ORIENTED_EDGE('',*,*,#2174,.F.);
#3026=ORIENTED_EDGE('',*,*,#2175,.F.);
#3027=ORIENTED_EDGE('',*,*,#2176,.F.);
#3028=ORIENTED_EDGE('',*,*,#2177,.F.);
#3029=ORIENTED_EDGE('',*,*,#2178,.F.);
#3030=ORIENTED_EDGE('',*,*,#2179,.F.);
#3031=ORIENTED_EDGE('',*,*,#2180,.F.);
#3032=ORIENTED_EDGE('',*,*,#2181,.F.);
#3033=ORIENTED_EDGE('',*,*,#2182,.F.);
#3034=ORIENTED_EDGE('',*,*,#2183,.F.);
#3035=ORIENTED_EDGE('',*,*,#2184,.F.);
#3036=ORIENTED_EDGE('',*,*,#2185,.F.);
#3037=ORIENTED_EDGE('',*,*,#2186,.T.);
#3038=ORIENTED_EDGE('',*,*,#2104,.T.);
#3039=ORIENTED_EDGE('',*,*,#2187,.T.);
#3040=ORIENTED_EDGE('',*,*,#2188,.F.);
#3041=ORIENTED_EDGE('',*,*,#2107,.T.);
#3042=ORIENTED_EDGE('',*,*,#2189,.F.);
#3043=ORIENTED_EDGE('',*,*,#2155,.T.);
#3044=ORIENTED_EDGE('',*,*,#2190,.T.);
#3045=ORIENTED_EDGE('',*,*,#2100,.T.);
#3046=ORIENTED_EDGE('',*,*,#2191,.T.);
#3047=ORIENTED_EDGE('',*,*,#2162,.T.);
#3048=ORIENTED_EDGE('',*,*,#2192,.F.);
#3049=ORIENTED_EDGE('',*,*,#2111,.T.);
#3050=ORIENTED_EDGE('',*,*,#2193,.F.);
#3051=ORIENTED_EDGE('',*,*,#2151,.T.);
#3052=ORIENTED_EDGE('',*,*,#2194,.T.);
#3053=ORIENTED_EDGE('',*,*,#2096,.T.);
#3054=ORIENTED_EDGE('',*,*,#2195,.T.);
#3055=ORIENTED_EDGE('',*,*,#2166,.T.);
#3056=ORIENTED_EDGE('',*,*,#2196,.F.);
#3057=ORIENTED_EDGE('',*,*,#2115,.T.);
#3058=ORIENTED_EDGE('',*,*,#2197,.F.);
#3059=ORIENTED_EDGE('',*,*,#2147,.T.);
#3060=ORIENTED_EDGE('',*,*,#2198,.T.);
#3061=ORIENTED_EDGE('',*,*,#2092,.T.);
#3062=ORIENTED_EDGE('',*,*,#2199,.T.);
#3063=ORIENTED_EDGE('',*,*,#2170,.T.);
#3064=ORIENTED_EDGE('',*,*,#2200,.F.);
#3065=ORIENTED_EDGE('',*,*,#2119,.T.);
#3066=ORIENTED_EDGE('',*,*,#2201,.F.);
#3067=ORIENTED_EDGE('',*,*,#2143,.T.);
#3068=ORIENTED_EDGE('',*,*,#2202,.T.);
#3069=ORIENTED_EDGE('',*,*,#2088,.T.);
#3070=ORIENTED_EDGE('',*,*,#2203,.T.);
#3071=ORIENTED_EDGE('',*,*,#2174,.T.);
#3072=ORIENTED_EDGE('',*,*,#2204,.F.);
#3073=ORIENTED_EDGE('',*,*,#2123,.T.);
#3074=ORIENTED_EDGE('',*,*,#2205,.F.);
#3075=ORIENTED_EDGE('',*,*,#2139,.T.);
#3076=ORIENTED_EDGE('',*,*,#2206,.T.);
#3077=ORIENTED_EDGE('',*,*,#2084,.T.);
#3078=ORIENTED_EDGE('',*,*,#2207,.T.);
#3079=ORIENTED_EDGE('',*,*,#2178,.T.);
#3080=ORIENTED_EDGE('',*,*,#2208,.F.);
#3081=ORIENTED_EDGE('',*,*,#2127,.T.);
#3082=ORIENTED_EDGE('',*,*,#2209,.F.);
#3083=ORIENTED_EDGE('',*,*,#2135,.T.);
#3084=ORIENTED_EDGE('',*,*,#2210,.T.);
#3085=ORIENTED_EDGE('',*,*,#2080,.T.);
#3086=ORIENTED_EDGE('',*,*,#2211,.T.);
#3087=ORIENTED_EDGE('',*,*,#2182,.T.);
#3088=ORIENTED_EDGE('',*,*,#2212,.F.);
#3089=ORIENTED_EDGE('',*,*,#2131,.T.);
#3090=ORIENTED_EDGE('',*,*,#2213,.F.);
#3091=ORIENTED_EDGE('',*,*,#2214,.F.);
#3092=ORIENTED_EDGE('',*,*,#2215,.T.);
#3093=ORIENTED_EDGE('',*,*,#2185,.T.);
#3094=ORIENTED_EDGE('',*,*,#2216,.F.);
#3095=ORIENTED_EDGE('',*,*,#2217,.F.);
#3096=ORIENTED_EDGE('',*,*,#2106,.T.);
#3097=ORIENTED_EDGE('',*,*,#2218,.F.);
#3098=ORIENTED_EDGE('',*,*,#2219,.F.);
#3099=ORIENTED_EDGE('',*,*,#2156,.T.);
#3100=ORIENTED_EDGE('',*,*,#2189,.T.);
#3101=ORIENTED_EDGE('',*,*,#2110,.T.);
#3102=ORIENTED_EDGE('',*,*,#2220,.F.);
#3103=ORIENTED_EDGE('',*,*,#2152,.T.);
#3104=ORIENTED_EDGE('',*,*,#2193,.T.);
#3105=ORIENTED_EDGE('',*,*,#2114,.T.);
#3106=ORIENTED_EDGE('',*,*,#2221,.F.);
#3107=ORIENTED_EDGE('',*,*,#2148,.T.);
#3108=ORIENTED_EDGE('',*,*,#2197,.T.);
#3109=ORIENTED_EDGE('',*,*,#2118,.T.);
#3110=ORIENTED_EDGE('',*,*,#2222,.F.);
#3111=ORIENTED_EDGE('',*,*,#2144,.T.);
#3112=ORIENTED_EDGE('',*,*,#2201,.T.);
#3113=ORIENTED_EDGE('',*,*,#2122,.T.);
#3114=ORIENTED_EDGE('',*,*,#2223,.F.);
#3115=ORIENTED_EDGE('',*,*,#2140,.T.);
#3116=ORIENTED_EDGE('',*,*,#2205,.T.);
#3117=ORIENTED_EDGE('',*,*,#2126,.T.);
#3118=ORIENTED_EDGE('',*,*,#2224,.F.);
#3119=ORIENTED_EDGE('',*,*,#2136,.T.);
#3120=ORIENTED_EDGE('',*,*,#2209,.T.);
#3121=ORIENTED_EDGE('',*,*,#2130,.T.);
#3122=ORIENTED_EDGE('',*,*,#2225,.F.);
#3123=ORIENTED_EDGE('',*,*,#2132,.T.);
#3124=ORIENTED_EDGE('',*,*,#2226,.F.);
#3125=ORIENTED_EDGE('',*,*,#2213,.T.);
#3126=ORIENTED_EDGE('',*,*,#2101,.T.);
#3127=ORIENTED_EDGE('',*,*,#2192,.T.);
#3128=ORIENTED_EDGE('',*,*,#2161,.T.);
#3129=ORIENTED_EDGE('',*,*,#2227,.F.);
#3130=ORIENTED_EDGE('',*,*,#2097,.T.);
#3131=ORIENTED_EDGE('',*,*,#2196,.T.);
#3132=ORIENTED_EDGE('',*,*,#2165,.T.);
#3133=ORIENTED_EDGE('',*,*,#2228,.F.);
#3134=ORIENTED_EDGE('',*,*,#2093,.T.);
#3135=ORIENTED_EDGE('',*,*,#2200,.T.);
#3136=ORIENTED_EDGE('',*,*,#2169,.T.);
#3137=ORIENTED_EDGE('',*,*,#2229,.F.);
#3138=ORIENTED_EDGE('',*,*,#2089,.T.);
#3139=ORIENTED_EDGE('',*,*,#2204,.T.);
#3140=ORIENTED_EDGE('',*,*,#2173,.T.);
#3141=ORIENTED_EDGE('',*,*,#2230,.F.);
#3142=ORIENTED_EDGE('',*,*,#2085,.T.);
#3143=ORIENTED_EDGE('',*,*,#2208,.T.);
#3144=ORIENTED_EDGE('',*,*,#2177,.T.);
#3145=ORIENTED_EDGE('',*,*,#2231,.F.);
#3146=ORIENTED_EDGE('',*,*,#2081,.T.);
#3147=ORIENTED_EDGE('',*,*,#2212,.T.);
#3148=ORIENTED_EDGE('',*,*,#2181,.T.);
#3149=ORIENTED_EDGE('',*,*,#2232,.F.);
#3150=ORIENTED_EDGE('',*,*,#2105,.T.);
#3151=ORIENTED_EDGE('',*,*,#2188,.T.);
#3152=ORIENTED_EDGE('',*,*,#2233,.T.);
#3153=ORIENTED_EDGE('',*,*,#2158,.T.);
#3154=ORIENTED_EDGE('',*,*,#2234,.T.);
#3155=ORIENTED_EDGE('',*,*,#2218,.T.);
#3156=ORIENTED_EDGE('',*,*,#2157,.T.);
#3157=ORIENTED_EDGE('',*,*,#2219,.T.);
#3158=ORIENTED_EDGE('',*,*,#2234,.F.);
#3159=ORIENTED_EDGE('',*,*,#2184,.T.);
#3160=ORIENTED_EDGE('',*,*,#2235,.T.);
#3161=ORIENTED_EDGE('',*,*,#2236,.F.);
#3162=ORIENTED_EDGE('',*,*,#2216,.T.);
#3163=ORIENTED_EDGE('',*,*,#2102,.T.);
#3164=ORIENTED_EDGE('',*,*,#2227,.T.);
#3165=ORIENTED_EDGE('',*,*,#2160,.T.);
#3166=ORIENTED_EDGE('',*,*,#2237,.T.);
#3167=ORIENTED_EDGE('',*,*,#2109,.T.);
#3168=ORIENTED_EDGE('',*,*,#2238,.T.);
#3169=ORIENTED_EDGE('',*,*,#2153,.T.);
#3170=ORIENTED_EDGE('',*,*,#2220,.T.);
#3171=ORIENTED_EDGE('',*,*,#2098,.T.);
#3172=ORIENTED_EDGE('',*,*,#2228,.T.);
#3173=ORIENTED_EDGE('',*,*,#2164,.T.);
#3174=ORIENTED_EDGE('',*,*,#2239,.T.);
#3175=ORIENTED_EDGE('',*,*,#2113,.T.);
#3176=ORIENTED_EDGE('',*,*,#2240,.T.);
#3177=ORIENTED_EDGE('',*,*,#2149,.T.);
#3178=ORIENTED_EDGE('',*,*,#2221,.T.);
#3179=ORIENTED_EDGE('',*,*,#2094,.T.);
#3180=ORIENTED_EDGE('',*,*,#2229,.T.);
#3181=ORIENTED_EDGE('',*,*,#2168,.T.);
#3182=ORIENTED_EDGE('',*,*,#2241,.T.);
#3183=ORIENTED_EDGE('',*,*,#2117,.T.);
#3184=ORIENTED_EDGE('',*,*,#2242,.T.);
#3185=ORIENTED_EDGE('',*,*,#2145,.T.);
#3186=ORIENTED_EDGE('',*,*,#2222,.T.);
#3187=ORIENTED_EDGE('',*,*,#2090,.T.);
#3188=ORIENTED_EDGE('',*,*,#2230,.T.);
#3189=ORIENTED_EDGE('',*,*,#2172,.T.);
#3190=ORIENTED_EDGE('',*,*,#2243,.T.);
#3191=ORIENTED_EDGE('',*,*,#2121,.T.);
#3192=ORIENTED_EDGE('',*,*,#2244,.T.);
#3193=ORIENTED_EDGE('',*,*,#2141,.T.);
#3194=ORIENTED_EDGE('',*,*,#2223,.T.);
#3195=ORIENTED_EDGE('',*,*,#2086,.T.);
#3196=ORIENTED_EDGE('',*,*,#2231,.T.);
#3197=ORIENTED_EDGE('',*,*,#2176,.T.);
#3198=ORIENTED_EDGE('',*,*,#2245,.T.);
#3199=ORIENTED_EDGE('',*,*,#2125,.T.);
#3200=ORIENTED_EDGE('',*,*,#2246,.T.);
#3201=ORIENTED_EDGE('',*,*,#2137,.T.);
#3202=ORIENTED_EDGE('',*,*,#2224,.T.);
#3203=ORIENTED_EDGE('',*,*,#2082,.T.);
#3204=ORIENTED_EDGE('',*,*,#2232,.T.);
#3205=ORIENTED_EDGE('',*,*,#2180,.T.);
#3206=ORIENTED_EDGE('',*,*,#2247,.T.);
#3207=ORIENTED_EDGE('',*,*,#2129,.T.);
#3208=ORIENTED_EDGE('',*,*,#2248,.T.);
#3209=ORIENTED_EDGE('',*,*,#2133,.T.);
#3210=ORIENTED_EDGE('',*,*,#2225,.T.);
#3211=ORIENTED_EDGE('',*,*,#2108,.T.);
#3212=ORIENTED_EDGE('',*,*,#2190,.F.);
#3213=ORIENTED_EDGE('',*,*,#2154,.T.);
#3214=ORIENTED_EDGE('',*,*,#2238,.F.);
#3215=ORIENTED_EDGE('',*,*,#2112,.T.);
#3216=ORIENTED_EDGE('',*,*,#2194,.F.);
#3217=ORIENTED_EDGE('',*,*,#2150,.T.);
#3218=ORIENTED_EDGE('',*,*,#2240,.F.);
#3219=ORIENTED_EDGE('',*,*,#2116,.T.);
#3220=ORIENTED_EDGE('',*,*,#2198,.F.);
#3221=ORIENTED_EDGE('',*,*,#2146,.T.);
#3222=ORIENTED_EDGE('',*,*,#2242,.F.);
#3223=ORIENTED_EDGE('',*,*,#2120,.T.);
#3224=ORIENTED_EDGE('',*,*,#2202,.F.);
#3225=ORIENTED_EDGE('',*,*,#2142,.T.);
#3226=ORIENTED_EDGE('',*,*,#2244,.F.);
#3227=ORIENTED_EDGE('',*,*,#2124,.T.);
#3228=ORIENTED_EDGE('',*,*,#2206,.F.);
#3229=ORIENTED_EDGE('',*,*,#2138,.T.);
#3230=ORIENTED_EDGE('',*,*,#2246,.F.);
#3231=ORIENTED_EDGE('',*,*,#2128,.T.);
#3232=ORIENTED_EDGE('',*,*,#2210,.F.);
#3233=ORIENTED_EDGE('',*,*,#2134,.T.);
#3234=ORIENTED_EDGE('',*,*,#2248,.F.);
#3235=ORIENTED_EDGE('',*,*,#2103,.T.);
#3236=ORIENTED_EDGE('',*,*,#2237,.F.);
#3237=ORIENTED_EDGE('',*,*,#2159,.T.);
#3238=ORIENTED_EDGE('',*,*,#2233,.F.);
#3239=ORIENTED_EDGE('',*,*,#2187,.F.);
#3240=ORIENTED_EDGE('',*,*,#2099,.T.);
#3241=ORIENTED_EDGE('',*,*,#2239,.F.);
#3242=ORIENTED_EDGE('',*,*,#2163,.T.);
#3243=ORIENTED_EDGE('',*,*,#2191,.F.);
#3244=ORIENTED_EDGE('',*,*,#2095,.T.);
#3245=ORIENTED_EDGE('',*,*,#2241,.F.);
#3246=ORIENTED_EDGE('',*,*,#2167,.T.);
#3247=ORIENTED_EDGE('',*,*,#2195,.F.);
#3248=ORIENTED_EDGE('',*,*,#2091,.T.);
#3249=ORIENTED_EDGE('',*,*,#2243,.F.);
#3250=ORIENTED_EDGE('',*,*,#2171,.T.);
#3251=ORIENTED_EDGE('',*,*,#2199,.F.);
#3252=ORIENTED_EDGE('',*,*,#2087,.T.);
#3253=ORIENTED_EDGE('',*,*,#2245,.F.);
#3254=ORIENTED_EDGE('',*,*,#2175,.T.);
#3255=ORIENTED_EDGE('',*,*,#2203,.F.);
#3256=ORIENTED_EDGE('',*,*,#2083,.T.);
#3257=ORIENTED_EDGE('',*,*,#2247,.F.);
#3258=ORIENTED_EDGE('',*,*,#2179,.T.);
#3259=ORIENTED_EDGE('',*,*,#2207,.F.);
#3260=ORIENTED_EDGE('',*,*,#2079,.T.);
#3261=ORIENTED_EDGE('',*,*,#2249,.F.);
#3262=ORIENTED_EDGE('',*,*,#2235,.F.);
#3263=ORIENTED_EDGE('',*,*,#2183,.T.);
#3264=ORIENTED_EDGE('',*,*,#2211,.F.);
#3265=ORIENTED_EDGE('',*,*,#2077,.T.);
#3266=ORIENTED_EDGE('',*,*,#2215,.F.);
#3267=ORIENTED_EDGE('',*,*,#2250,.F.);
#3268=ORIENTED_EDGE('',*,*,#2251,.F.);
#3269=ORIENTED_EDGE('',*,*,#2252,.T.);
#3270=ORIENTED_EDGE('',*,*,#2253,.F.);
#3271=ORIENTED_EDGE('',*,*,#2252,.F.);
#3272=ORIENTED_EDGE('',*,*,#2253,.T.);
#3273=ORIENTED_EDGE('',*,*,#2250,.T.);
#3274=ORIENTED_EDGE('',*,*,#2214,.T.);
#3275=ORIENTED_EDGE('',*,*,#2226,.T.);
#3276=ORIENTED_EDGE('',*,*,#2186,.F.);
#3277=ORIENTED_EDGE('',*,*,#2217,.T.);
#3278=ORIENTED_EDGE('',*,*,#2236,.T.);
#3279=ORIENTED_EDGE('',*,*,#2249,.T.);
#3280=ORIENTED_EDGE('',*,*,#2078,.F.);
#3281=ORIENTED_EDGE('',*,*,#2251,.T.);
#3282=ORIENTED_EDGE('',*,*,#2254,.F.);
#3283=ORIENTED_EDGE('',*,*,#2255,.T.);
#3284=ORIENTED_EDGE('',*,*,#2256,.T.);
#3285=ORIENTED_EDGE('',*,*,#2255,.F.);
#3286=ORIENTED_EDGE('',*,*,#2254,.T.);
#3287=ORIENTED_EDGE('',*,*,#2257,.F.);
#3288=ORIENTED_EDGE('',*,*,#2256,.F.);
#3289=ORIENTED_EDGE('',*,*,#2258,.T.);
#3290=ORIENTED_EDGE('',*,*,#2257,.T.);
#3291=ORIENTED_EDGE('',*,*,#2258,.F.);
#3292=ORIENTED_EDGE('',*,*,#2259,.T.);
#3293=ORIENTED_EDGE('',*,*,#2260,.T.);
#3294=ORIENTED_EDGE('',*,*,#2261,.T.);
#3295=ORIENTED_EDGE('',*,*,#2260,.F.);
#3296=ORIENTED_EDGE('',*,*,#2262,.F.);
#3297=ORIENTED_EDGE('',*,*,#2259,.F.);
#3298=ORIENTED_EDGE('',*,*,#2261,.F.);
#3299=ORIENTED_EDGE('',*,*,#2263,.T.);
#3300=ORIENTED_EDGE('',*,*,#2262,.T.);
#3301=ORIENTED_EDGE('',*,*,#2263,.F.);
#3302=ORIENTED_EDGE('',*,*,#2264,.F.);
#3303=ORIENTED_EDGE('',*,*,#2265,.T.);
#3304=ORIENTED_EDGE('',*,*,#2266,.F.);
#3305=ORIENTED_EDGE('',*,*,#2265,.F.);
#3306=ORIENTED_EDGE('',*,*,#2267,.F.);
#3307=ORIENTED_EDGE('',*,*,#2268,.T.);
#3308=ORIENTED_EDGE('',*,*,#2269,.T.);
#3309=ORIENTED_EDGE('',*,*,#2268,.F.);
#3310=ORIENTED_EDGE('',*,*,#2269,.F.);
#3311=ORIENTED_EDGE('',*,*,#2264,.T.);
#3312=ORIENTED_EDGE('',*,*,#2270,.F.);
#3313=ORIENTED_EDGE('',*,*,#2271,.T.);
#3314=ORIENTED_EDGE('',*,*,#2267,.T.);
#3315=ORIENTED_EDGE('',*,*,#2271,.F.);
#3316=ORIENTED_EDGE('',*,*,#2270,.T.);
#3317=ORIENTED_EDGE('',*,*,#2272,.T.);
#3318=ORIENTED_EDGE('',*,*,#2273,.F.);
#3319=ORIENTED_EDGE('',*,*,#2272,.F.);
#3320=ORIENTED_EDGE('',*,*,#2273,.T.);
#3321=ORIENTED_EDGE('',*,*,#2266,.T.);
#3322=ORIENTED_EDGE('',*,*,#2274,.T.);
#3323=ORIENTED_EDGE('',*,*,#2275,.T.);
#3324=ORIENTED_EDGE('',*,*,#2276,.F.);
#3325=ORIENTED_EDGE('',*,*,#2277,.F.);
#3326=ORIENTED_EDGE('',*,*,#2278,.T.);
#3327=ORIENTED_EDGE('',*,*,#2277,.T.);
#3328=ORIENTED_EDGE('',*,*,#2279,.F.);
#3329=ORIENTED_EDGE('',*,*,#2280,.F.);
#3330=ORIENTED_EDGE('',*,*,#2281,.T.);
#3331=ORIENTED_EDGE('',*,*,#2280,.T.);
#3332=ORIENTED_EDGE('',*,*,#2282,.F.);
#3333=ORIENTED_EDGE('',*,*,#2283,.F.);
#3334=ORIENTED_EDGE('',*,*,#2284,.T.);
#3335=ORIENTED_EDGE('',*,*,#2283,.T.);
#3336=ORIENTED_EDGE('',*,*,#2285,.F.);
#3337=ORIENTED_EDGE('',*,*,#2275,.F.);
#3338=ORIENTED_EDGE('',*,*,#2286,.T.);
#3339=ORIENTED_EDGE('',*,*,#2287,.T.);
#3340=ORIENTED_EDGE('',*,*,#2288,.F.);
#3341=ORIENTED_EDGE('',*,*,#2289,.F.);
#3342=ORIENTED_EDGE('',*,*,#2290,.T.);
#3343=ORIENTED_EDGE('',*,*,#2289,.T.);
#3344=ORIENTED_EDGE('',*,*,#2291,.F.);
#3345=ORIENTED_EDGE('',*,*,#2292,.F.);
#3346=ORIENTED_EDGE('',*,*,#2293,.T.);
#3347=ORIENTED_EDGE('',*,*,#2292,.T.);
#3348=ORIENTED_EDGE('',*,*,#2294,.F.);
#3349=ORIENTED_EDGE('',*,*,#2295,.F.);
#3350=ORIENTED_EDGE('',*,*,#2296,.T.);
#3351=ORIENTED_EDGE('',*,*,#2295,.T.);
#3352=ORIENTED_EDGE('',*,*,#2297,.F.);
#3353=ORIENTED_EDGE('',*,*,#2298,.F.);
#3354=ORIENTED_EDGE('',*,*,#2299,.T.);
#3355=ORIENTED_EDGE('',*,*,#2298,.T.);
#3356=ORIENTED_EDGE('',*,*,#2300,.F.);
#3357=ORIENTED_EDGE('',*,*,#2301,.F.);
#3358=ORIENTED_EDGE('',*,*,#2302,.T.);
#3359=ORIENTED_EDGE('',*,*,#2301,.T.);
#3360=ORIENTED_EDGE('',*,*,#2303,.F.);
#3361=ORIENTED_EDGE('',*,*,#2287,.F.);
#3362=ORIENTED_EDGE('',*,*,#2303,.T.);
#3363=ORIENTED_EDGE('',*,*,#2300,.T.);
#3364=ORIENTED_EDGE('',*,*,#2297,.T.);
#3365=ORIENTED_EDGE('',*,*,#2294,.T.);
#3366=ORIENTED_EDGE('',*,*,#2291,.T.);
#3367=ORIENTED_EDGE('',*,*,#2288,.T.);
#3368=ORIENTED_EDGE('',*,*,#2285,.T.);
#3369=ORIENTED_EDGE('',*,*,#2282,.T.);
#3370=ORIENTED_EDGE('',*,*,#2279,.T.);
#3371=ORIENTED_EDGE('',*,*,#2276,.T.);
#3372=ORIENTED_EDGE('',*,*,#2302,.F.);
#3373=ORIENTED_EDGE('',*,*,#2286,.F.);
#3374=ORIENTED_EDGE('',*,*,#2290,.F.);
#3375=ORIENTED_EDGE('',*,*,#2293,.F.);
#3376=ORIENTED_EDGE('',*,*,#2296,.F.);
#3377=ORIENTED_EDGE('',*,*,#2299,.F.);
#3378=ORIENTED_EDGE('',*,*,#2284,.F.);
#3379=ORIENTED_EDGE('',*,*,#2274,.F.);
#3380=ORIENTED_EDGE('',*,*,#2278,.F.);
#3381=ORIENTED_EDGE('',*,*,#2281,.F.);
#3382=ORIENTED_EDGE('',*,*,#2304,.F.);
#3383=ORIENTED_EDGE('',*,*,#2305,.F.);
#3384=ORIENTED_EDGE('',*,*,#2306,.F.);
#3385=ORIENTED_EDGE('',*,*,#2307,.T.);
#3386=ORIENTED_EDGE('',*,*,#2304,.T.);
#3387=ORIENTED_EDGE('',*,*,#2308,.T.);
#3388=ORIENTED_EDGE('',*,*,#2306,.T.);
#3389=ORIENTED_EDGE('',*,*,#2309,.F.);
#3390=ORIENTED_EDGE('',*,*,#2305,.T.);
#3391=ORIENTED_EDGE('',*,*,#2309,.T.);
#3392=ORIENTED_EDGE('',*,*,#2307,.F.);
#3393=ORIENTED_EDGE('',*,*,#2308,.F.);
#3394=CYLINDRICAL_SURFACE('',#3802,0.999999999999999);
#3395=CYLINDRICAL_SURFACE('',#3803,5.);
#3396=CYLINDRICAL_SURFACE('',#3811,7.52312685038423);
#3397=CYLINDRICAL_SURFACE('',#3817,7.52835105742136);
#3398=CYLINDRICAL_SURFACE('',#3823,6.40969108660508);
#3399=CYLINDRICAL_SURFACE('',#3829,6.41550316824698);
#3400=CYLINDRICAL_SURFACE('',#3835,6.40787078036307);
#3401=CYLINDRICAL_SURFACE('',#3839,6.40706623219228);
#3402=CYLINDRICAL_SURFACE('',#3845,4.66385643997278);
#3403=CYLINDRICAL_SURFACE('',#3849,3.44589712386029);
#3404=CYLINDRICAL_SURFACE('',#3852,1.77625);
#3405=CYLINDRICAL_SURFACE('',#3854,1.77625);
#3406=CYLINDRICAL_SURFACE('',#3855,1.77625);
#3407=CYLINDRICAL_SURFACE('',#3856,1.77625);
#3408=CYLINDRICAL_SURFACE('',#3857,1.77625);
#3409=CYLINDRICAL_SURFACE('',#3858,1.77625);
#3410=CYLINDRICAL_SURFACE('',#3859,1.77625);
#3411=CYLINDRICAL_SURFACE('',#3860,1.77625);
#3412=CYLINDRICAL_SURFACE('',#3861,1.77625);
#3413=CYLINDRICAL_SURFACE('',#3862,1.77625);
#3414=CYLINDRICAL_SURFACE('',#3863,1.77625);
#3415=CYLINDRICAL_SURFACE('',#3864,1.77625);
#3416=CYLINDRICAL_SURFACE('',#3865,1.77625);
#3417=CYLINDRICAL_SURFACE('',#3866,2.204);
#3418=CYLINDRICAL_SURFACE('',#3870,1.77625);
#3419=CYLINDRICAL_SURFACE('',#3891,4.48902817623056);
#3420=CYLINDRICAL_SURFACE('',#3944,4.42329516333974);
#3421=CYLINDRICAL_SURFACE('',#3945,2.21164758166987);
#3422=CYLINDRICAL_SURFACE('',#3946,2.21164758166987);
#3423=CYLINDRICAL_SURFACE('',#3948,4.433);
#3424=CYLINDRICAL_SURFACE('',#3951,3.72275);
#3425=CYLINDRICAL_SURFACE('',#3963,3.72275);
#3426=CYLINDRICAL_SURFACE('',#3965,3.72275);
#3427=CYLINDRICAL_SURFACE('',#3966,3.72275);
#3428=CYLINDRICAL_SURFACE('',#3967,3.72275);
#3429=CYLINDRICAL_SURFACE('',#3968,3.72275);
#3430=CYLINDRICAL_SURFACE('',#3969,3.72275);
#3431=CYLINDRICAL_SURFACE('',#3970,4.433);
#3432=CYLINDRICAL_SURFACE('',#3973,3.72275);
#3433=CYLINDRICAL_SURFACE('',#3975,1.77625);
#3434=CYLINDRICAL_SURFACE('',#3981,2.204);
#3435=CYLINDRICAL_SURFACE('',#3984,5.42440960677665);
#3436=CYLINDRICAL_SURFACE('',#4017,3.22275);
#3437=CYLINDRICAL_SURFACE('',#4019,3.22275);
#3438=CYLINDRICAL_SURFACE('',#4020,3.22275);
#3439=CYLINDRICAL_SURFACE('',#4021,3.22275);
#3440=CYLINDRICAL_SURFACE('',#4022,3.22275);
#3441=CYLINDRICAL_SURFACE('',#4023,3.22275);
#3442=CYLINDRICAL_SURFACE('',#4024,3.22275);
#3443=CYLINDRICAL_SURFACE('',#4025,3.22275);
#3444=CYLINDRICAL_SURFACE('',#4026,3.22275);
#3445=CYLINDRICAL_SURFACE('',#4027,3.22275);
#3446=CYLINDRICAL_SURFACE('',#4028,3.22275);
#3447=CYLINDRICAL_SURFACE('',#4029,3.22275);
#3448=CYLINDRICAL_SURFACE('',#4030,3.22275);
#3449=CYLINDRICAL_SURFACE('',#4031,3.22275);
#3450=CYLINDRICAL_SURFACE('',#4037,3.933);
#3451=CYLINDRICAL_SURFACE('',#4038,3.933);
#3452=CYLINDRICAL_SURFACE('',#4040,3.933);
#3453=CYLINDRICAL_SURFACE('',#4041,3.933);
#3454=CYLINDRICAL_SURFACE('',#4042,3.933);
#3455=CYLINDRICAL_SURFACE('',#4043,3.933);
#3456=CYLINDRICAL_SURFACE('',#4044,3.933);
#3457=CYLINDRICAL_SURFACE('',#4045,3.933);
#3458=CYLINDRICAL_SURFACE('',#4046,3.933);
#3459=CYLINDRICAL_SURFACE('',#4047,3.933);
#3460=CYLINDRICAL_SURFACE('',#4048,3.933);
#3461=CYLINDRICAL_SURFACE('',#4049,3.933);
#3462=CYLINDRICAL_SURFACE('',#4050,3.933);
#3463=CYLINDRICAL_SURFACE('',#4051,3.933);
#3464=CYLINDRICAL_SURFACE('',#4054,5.);
#3465=CYLINDRICAL_SURFACE('',#4060,4.88180150972878);
#3466=CYLINDRICAL_SURFACE('',#4073,4.88180150972878);
#3467=CYLINDRICAL_SURFACE('',#4074,2.204);
#3468=CYLINDRICAL_SURFACE('',#4081,7.52835105742136);
#3469=CYLINDRICAL_SURFACE('',#4087,4.433);
#3470=CYLINDRICAL_SURFACE('',#4090,3.72275);
#3471=ADVANCED_FACE('',(#379),#3394,.F.);
#3472=ADVANCED_FACE('',(#380),#3395,.F.);
#3473=ADVANCED_FACE('',(#381,#173),#203,.T.);
#3474=ADVANCED_FACE('',(#382),#155,.T.);
#3475=ADVANCED_FACE('',(#383,#174),#3396,.T.);
#3476=ADVANCED_FACE('',(#384),#156,.T.);
#3477=ADVANCED_FACE('',(#385),#157,.T.);
#3478=ADVANCED_FACE('',(#386),#3397,.T.);
#3479=ADVANCED_FACE('',(#387),#158,.T.);
#3480=ADVANCED_FACE('',(#388),#159,.F.);
#3481=ADVANCED_FACE('',(#389),#3398,.F.);
#3482=ADVANCED_FACE('',(#390),#160,.F.);
#3483=ADVANCED_FACE('',(#391,#175),#204,.T.);
#3484=ADVANCED_FACE('',(#392),#3399,.F.);
#3485=ADVANCED_FACE('',(#393,#176),#205,.T.);
#3486=ADVANCED_FACE('',(#394),#161,.F.);
#3487=ADVANCED_FACE('',(#395),#3400,.F.);
#3488=ADVANCED_FACE('',(#396),#162,.F.);
#3489=ADVANCED_FACE('',(#397),#3401,.F.);
#3490=ADVANCED_FACE('',(#398),#163,.F.);
#3491=ADVANCED_FACE('',(#399,#177),#206,.T.);
#3492=ADVANCED_FACE('',(#400),#3402,.F.);
#3493=ADVANCED_FACE('',(#401,#178),#207,.T.);
#3494=ADVANCED_FACE('',(#402,#179),#3403,.F.);
#3495=ADVANCED_FACE('',(#403,#180),#208,.T.);
#3496=ADVANCED_FACE('',(#404),#3404,.T.);
#3497=ADVANCED_FACE('',(#405),#3405,.T.);
#3498=ADVANCED_FACE('',(#406),#3406,.T.);
#3499=ADVANCED_FACE('',(#407),#3407,.T.);
#3500=ADVANCED_FACE('',(#408),#3408,.T.);
#3501=ADVANCED_FACE('',(#409),#3409,.T.);
#3502=ADVANCED_FACE('',(#410),#3410,.T.);
#3503=ADVANCED_FACE('',(#411),#3411,.T.);
#3504=ADVANCED_FACE('',(#412),#3412,.T.);
#3505=ADVANCED_FACE('',(#413),#3413,.T.);
#3506=ADVANCED_FACE('',(#414),#3414,.T.);
#3507=ADVANCED_FACE('',(#415),#3415,.T.);
#3508=ADVANCED_FACE('',(#416),#3416,.T.);
#3509=ADVANCED_FACE('',(#417,#181),#3417,.T.);
#3510=ADVANCED_FACE('',(#418),#3418,.T.);
#3511=ADVANCED_FACE('',(#419,#182),#209,.T.);
#3512=ADVANCED_FACE('',(#420),#98,.T.);
#3513=ADVANCED_FACE('',(#421),#164,.T.);
#3514=ADVANCED_FACE('',(#422),#99,.T.);
#3515=ADVANCED_FACE('',(#423,#183),#210,.T.);
#3516=ADVANCED_FACE('',(#424),#58,.F.);
#3517=ADVANCED_FACE('',(#425),#211,.T.);
#3518=ADVANCED_FACE('',(#426),#59,.F.);
#3519=ADVANCED_FACE('',(#427),#212,.T.);
#3520=ADVANCED_FACE('',(#428),#100,.T.);
#3521=ADVANCED_FACE('',(#429),#3419,.T.);
#3522=ADVANCED_FACE('',(#430,#184),#213,.T.);
#3523=ADVANCED_FACE('',(#431),#101,.T.);
#3524=ADVANCED_FACE('',(#432),#165,.T.);
#3525=ADVANCED_FACE('',(#433,#185),#214,.T.);
#3526=ADVANCED_FACE('',(#434),#102,.T.);
#3527=ADVANCED_FACE('',(#435,#186),#215,.T.);
#3528=ADVANCED_FACE('',(#436),#103,.T.);
#3529=ADVANCED_FACE('',(#437),#166,.T.);
#3530=ADVANCED_FACE('',(#438,#187),#216,.T.);
#3531=ADVANCED_FACE('',(#439),#104,.T.);
#3532=ADVANCED_FACE('',(#440),#105,.T.);
#3533=ADVANCED_FACE('',(#441),#167,.T.);
#3534=ADVANCED_FACE('',(#442),#106,.T.);
#3535=ADVANCED_FACE('',(#443,#188),#217,.T.);
#3536=ADVANCED_FACE('',(#444),#107,.T.);
#3537=ADVANCED_FACE('',(#445),#168,.T.);
#3538=ADVANCED_FACE('',(#446,#189),#218,.T.);
#3539=ADVANCED_FACE('',(#447),#108,.T.);
#3540=ADVANCED_FACE('',(#448,#190),#219,.T.);
#3541=ADVANCED_FACE('',(#449),#109,.T.);
#3542=ADVANCED_FACE('',(#450),#220,.T.);
#3543=ADVANCED_FACE('',(#451),#3420,.T.);
#3544=ADVANCED_FACE('',(#452),#3421,.T.);
#3545=ADVANCED_FACE('',(#453),#3422,.T.);
#3546=ADVANCED_FACE('',(#454),#60,.T.);
#3547=ADVANCED_FACE('',(#455),#3423,.F.);
#3548=ADVANCED_FACE('',(#456),#61,.T.);
#3549=ADVANCED_FACE('',(#457),#3424,.F.);
#3550=ADVANCED_FACE('',(#458),#221,.T.);
#3551=ADVANCED_FACE('',(#459),#222,.T.);
#3552=ADVANCED_FACE('',(#460),#223,.T.);
#3553=ADVANCED_FACE('',(#461),#224,.T.);
#3554=ADVANCED_FACE('',(#462),#225,.T.);
#3555=ADVANCED_FACE('',(#463),#226,.T.);
#3556=ADVANCED_FACE('',(#464,#191),#227,.T.);
#3557=ADVANCED_FACE('',(#465,#192),#228,.F.);
#3558=ADVANCED_FACE('',(#466),#3425,.T.);
#3559=ADVANCED_FACE('',(#467),#3426,.T.);
#3560=ADVANCED_FACE('',(#468),#3427,.T.);
#3561=ADVANCED_FACE('',(#469),#3428,.T.);
#3562=ADVANCED_FACE('',(#470),#3429,.T.);
#3563=ADVANCED_FACE('',(#471),#3430,.T.);
#3564=ADVANCED_FACE('',(#472),#3431,.T.);
#3565=ADVANCED_FACE('',(#473),#3432,.T.);
#3566=ADVANCED_FACE('',(#474),#62,.T.);
#3567=ADVANCED_FACE('',(#475),#3433,.F.);
#3568=ADVANCED_FACE('',(#476),#63,.T.);
#3569=ADVANCED_FACE('',(#477),#229,.F.);
#3570=ADVANCED_FACE('',(#478),#3434,.F.);
#3571=ADVANCED_FACE('',(#479),#64,.F.);
#3572=ADVANCED_FACE('',(#480),#65,.F.);
#3573=ADVANCED_FACE('',(#481),#3435,.T.);
#3574=ADVANCED_FACE('',(#482,#193),#230,.T.);
#3575=ADVANCED_FACE('',(#483,#194),#231,.T.);
#3576=ADVANCED_FACE('',(#484,#195),#232,.F.);
#3577=ADVANCED_FACE('',(#485),#110,.T.);
#3578=ADVANCED_FACE('',(#486),#169,.T.);
#3579=ADVANCED_FACE('',(#487),#233,.T.);
#3580=ADVANCED_FACE('',(#488),#111,.T.);
#3581=ADVANCED_FACE('',(#489),#234,.T.);
#3582=ADVANCED_FACE('',(#490),#112,.T.);
#3583=ADVANCED_FACE('',(#491),#170,.T.);
#3584=ADVANCED_FACE('',(#492),#235,.T.);
#3585=ADVANCED_FACE('',(#493),#113,.T.);
#3586=ADVANCED_FACE('',(#494),#236,.T.);
#3587=ADVANCED_FACE('',(#495),#237,.F.);
#3588=ADVANCED_FACE('',(#496),#238,.F.);
#3589=ADVANCED_FACE('',(#497),#3436,.T.);
#3590=ADVANCED_FACE('',(#498),#3437,.T.);
#3591=ADVANCED_FACE('',(#499),#3438,.T.);
#3592=ADVANCED_FACE('',(#500),#3439,.T.);
#3593=ADVANCED_FACE('',(#501),#3440,.T.);
#3594=ADVANCED_FACE('',(#502),#3441,.T.);
#3595=ADVANCED_FACE('',(#503),#3442,.T.);
#3596=ADVANCED_FACE('',(#504),#3443,.T.);
#3597=ADVANCED_FACE('',(#505),#3444,.T.);
#3598=ADVANCED_FACE('',(#506),#3445,.T.);
#3599=ADVANCED_FACE('',(#507),#3446,.T.);
#3600=ADVANCED_FACE('',(#508),#3447,.T.);
#3601=ADVANCED_FACE('',(#509),#3448,.T.);
#3602=ADVANCED_FACE('',(#510),#3449,.T.);
#3603=ADVANCED_FACE('',(#511),#66,.F.);
#3604=ADVANCED_FACE('',(#512),#67,.F.);
#3605=ADVANCED_FACE('',(#513),#68,.F.);
#3606=ADVANCED_FACE('',(#514),#69,.F.);
#3607=ADVANCED_FACE('',(#515),#70,.F.);
#3608=ADVANCED_FACE('',(#516),#71,.F.);
#3609=ADVANCED_FACE('',(#517),#72,.F.);
#3610=ADVANCED_FACE('',(#518),#73,.F.);
#3611=ADVANCED_FACE('',(#519),#74,.F.);
#3612=ADVANCED_FACE('',(#520),#75,.F.);
#3613=ADVANCED_FACE('',(#521),#76,.F.);
#3614=ADVANCED_FACE('',(#522),#77,.F.);
#3615=ADVANCED_FACE('',(#523),#78,.F.);
#3616=ADVANCED_FACE('',(#524),#79,.F.);
#3617=ADVANCED_FACE('',(#525),#239,.T.);
#3618=ADVANCED_FACE('',(#526),#3450,.T.);
#3619=ADVANCED_FACE('',(#527),#3451,.T.);
#3620=ADVANCED_FACE('',(#528),#3452,.T.);
#3621=ADVANCED_FACE('',(#529),#3453,.T.);
#3622=ADVANCED_FACE('',(#530),#3454,.T.);
#3623=ADVANCED_FACE('',(#531),#3455,.T.);
#3624=ADVANCED_FACE('',(#532),#3456,.T.);
#3625=ADVANCED_FACE('',(#533),#3457,.T.);
#3626=ADVANCED_FACE('',(#534),#3458,.T.);
#3627=ADVANCED_FACE('',(#535),#3459,.T.);
#3628=ADVANCED_FACE('',(#536),#3460,.T.);
#3629=ADVANCED_FACE('',(#537),#3461,.T.);
#3630=ADVANCED_FACE('',(#538),#3462,.T.);
#3631=ADVANCED_FACE('',(#539),#3463,.T.);
#3632=ADVANCED_FACE('',(#540),#80,.F.);
#3633=ADVANCED_FACE('',(#541),#81,.F.);
#3634=ADVANCED_FACE('',(#542),#82,.F.);
#3635=ADVANCED_FACE('',(#543),#83,.F.);
#3636=ADVANCED_FACE('',(#544),#84,.F.);
#3637=ADVANCED_FACE('',(#545),#85,.F.);
#3638=ADVANCED_FACE('',(#546),#86,.F.);
#3639=ADVANCED_FACE('',(#547),#87,.F.);
#3640=ADVANCED_FACE('',(#548),#88,.F.);
#3641=ADVANCED_FACE('',(#549),#89,.F.);
#3642=ADVANCED_FACE('',(#550),#90,.F.);
#3643=ADVANCED_FACE('',(#551),#91,.F.);
#3644=ADVANCED_FACE('',(#552),#92,.F.);
#3645=ADVANCED_FACE('',(#553),#93,.F.);
#3646=ADVANCED_FACE('',(#554),#3464,.T.);
#3647=ADVANCED_FACE('',(#555,#196),#240,.T.);
#3648=ADVANCED_FACE('',(#556),#241,.F.);
#3649=ADVANCED_FACE('',(#557),#3465,.F.);
#3650=ADVANCED_FACE('',(#558,#197),#242,.T.);
#3651=ADVANCED_FACE('',(#559),#114,.T.);
#3652=ADVANCED_FACE('',(#560),#115,.T.);
#3653=ADVANCED_FACE('',(#561,#198),#243,.T.);
#3654=ADVANCED_FACE('',(#562),#3466,.F.);
#3655=ADVANCED_FACE('',(#563),#3467,.F.);
#3656=ADVANCED_FACE('',(#564),#171,.T.);
#3657=ADVANCED_FACE('',(#565,#199),#244,.T.);
#3658=ADVANCED_FACE('',(#566),#3468,.T.);
#3659=ADVANCED_FACE('',(#567),#172,.T.);
#3660=ADVANCED_FACE('',(#568,#200),#245,.T.);
#3661=ADVANCED_FACE('',(#569),#94,.T.);
#3662=ADVANCED_FACE('',(#570),#3469,.F.);
#3663=ADVANCED_FACE('',(#571),#95,.T.);
#3664=ADVANCED_FACE('',(#572),#3470,.F.);
#3665=ADVANCED_FACE('',(#573),#246,.T.);
#3666=ADVANCED_FACE('',(#574),#247,.T.);
#3667=ADVANCED_FACE('',(#575),#248,.T.);
#3668=ADVANCED_FACE('',(#576),#249,.T.);
#3669=ADVANCED_FACE('',(#577),#250,.T.);
#3670=ADVANCED_FACE('',(#578),#251,.T.);
#3671=ADVANCED_FACE('',(#579,#201),#252,.T.);
#3672=ADVANCED_FACE('',(#580,#202),#253,.F.);
#3673=ADVANCED_FACE('',(#581),#96,.T.);
#3674=ADVANCED_FACE('',(#582),#97,.T.);
#3675=ADVANCED_FACE('',(#583),#254,.T.);
#3676=ADVANCED_FACE('',(#584),#255,.F.);
#3677=CLOSED_SHELL('',(#3471,#3472,#3473,#3474,#3475,#3476,#3477,#3478,
#3479,#3480,#3481,#3482,#3483,#3484,#3485,#3486,#3487,#3488,#3489,#3490,
#3491,#3492,#3493,#3494,#3495));
#3678=CLOSED_SHELL('',(#3496,#3497,#3498,#3499,#3500,#3501,#3502,#3503,
#3504,#3505,#3506,#3507,#3508,#3509,#3510,#3511,#3512,#3513,#3514,#3515,
#3516,#3517,#3518,#3519,#3520,#3521,#3522,#3523,#3524,#3525,#3526,#3527,
#3528,#3529,#3530,#3531,#3532,#3533,#3534,#3535,#3536,#3537,#3538,#3539,
#3540,#3541,#3542,#3543,#3544,#3545));
#3679=CLOSED_SHELL('',(#3546,#3547,#3548,#3549,#3550,#3551,#3552,#3553,
#3554,#3555,#3556,#3557));
#3680=CLOSED_SHELL('',(#3558,#3559,#3560,#3561,#3562,#3563,#3564,#3565,
#3566,#3567,#3568,#3569,#3570,#3571,#3572,#3573,#3574,#3575,#3576));
#3681=CLOSED_SHELL('',(#3577,#3578,#3579,#3580,#3581));
#3682=CLOSED_SHELL('',(#3582,#3583,#3584,#3585,#3586));
#3683=CLOSED_SHELL('',(#3587,#3588,#3589,#3590,#3591,#3592,#3593,#3594,
#3595,#3596,#3597,#3598,#3599,#3600,#3601,#3602,#3603,#3604,#3605,#3606,
#3607,#3608,#3609,#3610,#3611,#3612,#3613,#3614,#3615,#3616,#3617,#3618,
#3619,#3620,#3621,#3622,#3623,#3624,#3625,#3626,#3627,#3628,#3629,#3630,
#3631,#3632,#3633,#3634,#3635,#3636,#3637,#3638,#3639,#3640,#3641,#3642,
#3643,#3644,#3645,#3646,#3647,#3648));
#3684=CLOSED_SHELL('',(#3649,#3650,#3651));
#3685=CLOSED_SHELL('',(#3652,#3653,#3654));
#3686=CLOSED_SHELL('',(#3655,#3656,#3657,#3658,#3659,#3660));
#3687=CLOSED_SHELL('',(#3661,#3662,#3663,#3664,#3665,#3666,#3667,#3668,
#3669,#3670,#3671,#3672));
#3688=CLOSED_SHELL('',(#3673,#3674,#3675,#3676));
#3689=DERIVED_UNIT_ELEMENT(#3709,1.);
#3690=DERIVED_UNIT_ELEMENT(#28057,-3.);
#3691=DERIVED_UNIT_ELEMENT(#3709,1.);
#3692=DERIVED_UNIT_ELEMENT(#28057,-3.);
#3693=DERIVED_UNIT_ELEMENT(#3709,1.);
#3694=DERIVED_UNIT_ELEMENT(#28057,-3.);
#3695=DERIVED_UNIT_ELEMENT(#3709,1.);
#3696=DERIVED_UNIT_ELEMENT(#28057,-3.);
#3697=DERIVED_UNIT_ELEMENT(#3709,1.);
#3698=DERIVED_UNIT_ELEMENT(#28057,-3.);
#3699=DERIVED_UNIT_ELEMENT(#3709,1.);
#3700=DERIVED_UNIT_ELEMENT(#28057,-3.);
#3701=DERIVED_UNIT_ELEMENT(#3709,1.);
#3702=DERIVED_UNIT_ELEMENT(#28057,-3.);
#3703=DERIVED_UNIT_ELEMENT(#3709,1.);
#3704=DERIVED_UNIT_ELEMENT(#28057,-3.);
#3705=DERIVED_UNIT_ELEMENT(#3709,1.);
#3706=DERIVED_UNIT_ELEMENT(#28057,-3.);
#3707=DERIVED_UNIT_ELEMENT(#3709,1.);
#3708=DERIVED_UNIT_ELEMENT(#28057,-3.);
#3709=(
MASS_UNIT()
NAMED_UNIT(*)
SI_UNIT(.KILO.,.GRAM.)
);
#3710=DERIVED_UNIT((#3689,#3690));
#3711=DERIVED_UNIT((#3691,#3692));
#3712=DERIVED_UNIT((#3693,#3694));
#3713=DERIVED_UNIT((#3695,#3696));
#3714=DERIVED_UNIT((#3697,#3698));
#3715=DERIVED_UNIT((#3699,#3700));
#3716=DERIVED_UNIT((#3701,#3702));
#3717=DERIVED_UNIT((#3703,#3704));
#3718=DERIVED_UNIT((#3705,#3706));
#3719=DERIVED_UNIT((#3707,#3708));
#3720=MEASURE_REPRESENTATION_ITEM('density measure',
POSITIVE_RATIO_MEASURE(7850.),#3710);
#3721=MEASURE_REPRESENTATION_ITEM('density measure',
POSITIVE_RATIO_MEASURE(7850.),#3711);
#3722=MEASURE_REPRESENTATION_ITEM('density measure',
POSITIVE_RATIO_MEASURE(7850.),#3712);
#3723=MEASURE_REPRESENTATION_ITEM('density measure',
POSITIVE_RATIO_MEASURE(7850.),#3713);
#3724=MEASURE_REPRESENTATION_ITEM('density measure',
POSITIVE_RATIO_MEASURE(930.),#3714);
#3725=MEASURE_REPRESENTATION_ITEM('density measure',
POSITIVE_RATIO_MEASURE(930.),#3715);
#3726=MEASURE_REPRESENTATION_ITEM('density measure',
POSITIVE_RATIO_MEASURE(7850.),#3716);
#3727=MEASURE_REPRESENTATION_ITEM('density measure',
POSITIVE_RATIO_MEASURE(7850.),#3717);
#3728=MEASURE_REPRESENTATION_ITEM('density measure',
POSITIVE_RATIO_MEASURE(7850.),#3718);
#3729=MEASURE_REPRESENTATION_ITEM('density measure',
POSITIVE_RATIO_MEASURE(7850.),#3719);
#3730=PROPERTY_DEFINITION_REPRESENTATION(#3780,#3750);
#3731=PROPERTY_DEFINITION_REPRESENTATION(#3781,#3751);
#3732=PROPERTY_DEFINITION_REPRESENTATION(#3782,#3752);
#3733=PROPERTY_DEFINITION_REPRESENTATION(#3783,#3753);
#3734=PROPERTY_DEFINITION_REPRESENTATION(#3784,#3754);
#3735=PROPERTY_DEFINITION_REPRESENTATION(#3785,#3755);
#3736=PROPERTY_DEFINITION_REPRESENTATION(#3786,#3756);
#3737=PROPERTY_DEFINITION_REPRESENTATION(#3787,#3757);
#3738=PROPERTY_DEFINITION_REPRESENTATION(#3788,#3758);
#3739=PROPERTY_DEFINITION_REPRESENTATION(#3789,#3759);
#3740=PROPERTY_DEFINITION_REPRESENTATION(#3790,#3760);
#3741=PROPERTY_DEFINITION_REPRESENTATION(#3791,#3761);
#3742=PROPERTY_DEFINITION_REPRESENTATION(#3792,#3762);
#3743=PROPERTY_DEFINITION_REPRESENTATION(#3793,#3763);
#3744=PROPERTY_DEFINITION_REPRESENTATION(#3794,#3764);
#3745=PROPERTY_DEFINITION_REPRESENTATION(#3795,#3765);
#3746=PROPERTY_DEFINITION_REPRESENTATION(#3796,#3766);
#3747=PROPERTY_DEFINITION_REPRESENTATION(#3797,#3767);
#3748=PROPERTY_DEFINITION_REPRESENTATION(#3798,#3768);
#3749=PROPERTY_DEFINITION_REPRESENTATION(#3799,#3769);
#3750=REPRESENTATION('material name',(#3770),#28045);
#3751=REPRESENTATION('density',(#3720),#28045);
#3752=REPRESENTATION('material name',(#3771),#28046);
#3753=REPRESENTATION('density',(#3721),#28046);
#3754=REPRESENTATION('material name',(#3772),#28047);
#3755=REPRESENTATION('density',(#3722),#28047);
#3756=REPRESENTATION('material name',(#3773),#28048);
#3757=REPRESENTATION('density',(#3723),#28048);
#3758=REPRESENTATION('material name',(#3774),#28049);
#3759=REPRESENTATION('density',(#3724),#28049);
#3760=REPRESENTATION('material name',(#3775),#28050);
#3761=REPRESENTATION('density',(#3725),#28050);
#3762=REPRESENTATION('material name',(#3776),#28051);
#3763=REPRESENTATION('density',(#3726),#28051);
#3764=REPRESENTATION('material name',(#3777),#28052);
#3765=REPRESENTATION('density',(#3727),#28052);
#3766=REPRESENTATION('material name',(#3778),#28053);
#3767=REPRESENTATION('density',(#3728),#28053);
#3768=REPRESENTATION('material name',(#3779),#28054);
#3769=REPRESENTATION('density',(#3729),#28054);
#3770=DESCRIPTIVE_REPRESENTATION_ITEM('Steel','Steel');
#3771=DESCRIPTIVE_REPRESENTATION_ITEM('Steel','Steel');
#3772=DESCRIPTIVE_REPRESENTATION_ITEM('Steel','Steel');
#3773=DESCRIPTIVE_REPRESENTATION_ITEM('Steel','Steel');
#3774=DESCRIPTIVE_REPRESENTATION_ITEM('Rubber','Rubber');
#3775=DESCRIPTIVE_REPRESENTATION_ITEM('Rubber','Rubber');
#3776=DESCRIPTIVE_REPRESENTATION_ITEM('Steel','Steel');
#3777=DESCRIPTIVE_REPRESENTATION_ITEM('Steel','Steel');
#3778=DESCRIPTIVE_REPRESENTATION_ITEM('Steel','Steel');
#3779=DESCRIPTIVE_REPRESENTATION_ITEM('Steel','Steel');
#3780=PROPERTY_DEFINITION('material property','material name',#28105);
#3781=PROPERTY_DEFINITION('material property','density of part',#28105);
#3782=PROPERTY_DEFINITION('material property','material name',#28106);
#3783=PROPERTY_DEFINITION('material property','density of part',#28106);
#3784=PROPERTY_DEFINITION('material property','material name',#28107);
#3785=PROPERTY_DEFINITION('material property','density of part',#28107);
#3786=PROPERTY_DEFINITION('material property','material name',#28108);
#3787=PROPERTY_DEFINITION('material property','density of part',#28108);
#3788=PROPERTY_DEFINITION('material property','material name',#28109);
#3789=PROPERTY_DEFINITION('material property','density of part',#28109);
#3790=PROPERTY_DEFINITION('material property','material name',#28110);
#3791=PROPERTY_DEFINITION('material property','density of part',#28110);
#3792=PROPERTY_DEFINITION('material property','material name',#28111);
#3793=PROPERTY_DEFINITION('material property','density of part',#28111);
#3794=PROPERTY_DEFINITION('material property','material name',#28112);
#3795=PROPERTY_DEFINITION('material property','density of part',#28112);
#3796=PROPERTY_DEFINITION('material property','material name',#28113);
#3797=PROPERTY_DEFINITION('material property','density of part',#28113);
#3798=PROPERTY_DEFINITION('material property','material name',#28114);
#3799=PROPERTY_DEFINITION('material property','density of part',#28114);
#3800=AXIS2_PLACEMENT_3D('',#4900,#4114,#4115);
#3801=AXIS2_PLACEMENT_3D('',#4901,#4116,#4117);
#3802=AXIS2_PLACEMENT_3D('',#4902,#4118,#4119);
#3803=AXIS2_PLACEMENT_3D('',#4980,#4121,#4122);
#3804=AXIS2_PLACEMENT_3D('',#4982,#4123,#4124);
#3805=AXIS2_PLACEMENT_3D('',#4985,#4126,#4127);
#3806=AXIS2_PLACEMENT_3D('',#4986,#4128,#4129);
#3807=AXIS2_PLACEMENT_3D('',#4988,#4130,#4131);
#3808=AXIS2_PLACEMENT_3D('',#4989,#4132,#4133);
#3809=AXIS2_PLACEMENT_3D('',#4991,#4134,#4135);
#3810=AXIS2_PLACEMENT_3D('',#4994,#4137,#4138);
#3811=AXIS2_PLACEMENT_3D('',#4995,#4139,#4140);
#3812=AXIS2_PLACEMENT_3D('',#4997,#4141,#4142);
#3813=AXIS2_PLACEMENT_3D('',#4999,#4144,#4145);
#3814=AXIS2_PLACEMENT_3D('',#5002,#4147,#4148);
#3815=AXIS2_PLACEMENT_3D('',#5003,#4149,#4150);
#3816=AXIS2_PLACEMENT_3D('',#5005,#4151,#4152);
#3817=AXIS2_PLACEMENT_3D('',#5007,#4154,#4155);
#3818=AXIS2_PLACEMENT_3D('',#5009,#4156,#4157);
#3819=AXIS2_PLACEMENT_3D('',#5011,#4159,#4160);
#3820=AXIS2_PLACEMENT_3D('',#5014,#4162,#4163);
#3821=AXIS2_PLACEMENT_3D('',#5015,#4164,#4165);
#3822=AXIS2_PLACEMENT_3D('',#5017,#4166,#4167);
#3823=AXIS2_PLACEMENT_3D('',#5019,#4169,#4170);
#3824=AXIS2_PLACEMENT_3D('',#5021,#4171,#4172);
#3825=AXIS2_PLACEMENT_3D('',#5023,#4174,#4175);
#3826=AXIS2_PLACEMENT_3D('',#5025,#4176,#4177);
#3827=AXIS2_PLACEMENT_3D('',#5027,#4179,#4180);
#3828=AXIS2_PLACEMENT_3D('',#5029,#4181,#4182);
#3829=AXIS2_PLACEMENT_3D('',#5030,#4183,#4184);
#3830=AXIS2_PLACEMENT_3D('',#5032,#4185,#4186);
#3831=AXIS2_PLACEMENT_3D('',#5034,#4188,#4189);
#3832=AXIS2_PLACEMENT_3D('',#5036,#4190,#4191);
#3833=AXIS2_PLACEMENT_3D('',#5037,#4192,#4193);
#3834=AXIS2_PLACEMENT_3D('',#5039,#4194,#4195);
#3835=AXIS2_PLACEMENT_3D('',#5041,#4197,#4198);
#3836=AXIS2_PLACEMENT_3D('',#5043,#4199,#4200);
#3837=AXIS2_PLACEMENT_3D('',#5045,#4202,#4203);
#3838=AXIS2_PLACEMENT_3D('',#5047,#4204,#4205);
#3839=AXIS2_PLACEMENT_3D('',#5049,#4207,#4208);
#3840=AXIS2_PLACEMENT_3D('',#5051,#4209,#4210);
#3841=AXIS2_PLACEMENT_3D('',#5053,#4212,#4213);
#3842=AXIS2_PLACEMENT_3D('',#5055,#4214,#4215);
#3843=AXIS2_PLACEMENT_3D('',#5057,#4217,#4218);
#3844=AXIS2_PLACEMENT_3D('',#5059,#4219,#4220);
#3845=AXIS2_PLACEMENT_3D('',#5060,#4221,#4222);
#3846=AXIS2_PLACEMENT_3D('',#5062,#4223,#4224);
#3847=AXIS2_PLACEMENT_3D('',#5064,#4226,#4227);
#3848=AXIS2_PLACEMENT_3D('',#5066,#4228,#4229);
#3849=AXIS2_PLACEMENT_3D('',#5067,#4230,#4231);
#3850=AXIS2_PLACEMENT_3D('',#5069,#4233,#4234);
#3851=AXIS2_PLACEMENT_3D('',#5070,#4235,#4236);
#3852=AXIS2_PLACEMENT_3D('',#5071,#4237,#4238);
#3853=AXIS2_PLACEMENT_3D('',#5233,#4240,#4241);
#3854=AXIS2_PLACEMENT_3D('',#5343,#4242,#4243);
#3855=AXIS2_PLACEMENT_3D('',#5733,#4245,#4246);
#3856=AXIS2_PLACEMENT_3D('',#5859,#4248,#4249);
#3857=AXIS2_PLACEMENT_3D('',#6170,#4251,#4252);
#3858=AXIS2_PLACEMENT_3D('',#6558,#4254,#4255);
#3859=AXIS2_PLACEMENT_3D('',#6957,#4257,#4258);
#3860=AXIS2_PLACEMENT_3D('',#7344,#4260,#4261);
#3861=AXIS2_PLACEMENT_3D('',#7745,#4263,#4264);
#3862=AXIS2_PLACEMENT_3D('',#8140,#4266,#4267);
#3863=AXIS2_PLACEMENT_3D('',#8549,#4269,#4270);
#3864=AXIS2_PLACEMENT_3D('',#8952,#4272,#4273);
#3865=AXIS2_PLACEMENT_3D('',#9334,#4275,#4276);
#3866=AXIS2_PLACEMENT_3D('',#9453,#4278,#4279);
#3867=AXIS2_PLACEMENT_3D('',#9455,#4280,#4281);
#3868=AXIS2_PLACEMENT_3D('',#9458,#4282,#4283);
#3869=AXIS2_PLACEMENT_3D('',#11773,#4284,#4285);
#3870=AXIS2_PLACEMENT_3D('',#14184,#4286,#4287);
#3871=AXIS2_PLACEMENT_3D('',#14284,#4288,#4289);
#3872=AXIS2_PLACEMENT_3D('',#14344,#4290,#4291);
#3873=AXIS2_PLACEMENT_3D('',#14346,#4292,#4293);
#3874=AXIS2_PLACEMENT_3D('',#14348,#4294,#4295);
#3875=AXIS2_PLACEMENT_3D('',#14349,#4296,#4297);
#3876=AXIS2_PLACEMENT_3D('',#14351,#4298,#4299);
#3877=AXIS2_PLACEMENT_3D('',#14353,#4300,#4301);
#3878=AXIS2_PLACEMENT_3D('',#14354,#4302,#4303);
#3879=AXIS2_PLACEMENT_3D('',#14355,#4304,#4305);
#3880=AXIS2_PLACEMENT_3D('',#14358,#4307,#4308);
#3881=AXIS2_PLACEMENT_3D('',#14359,#4309,#4310);
#3882=AXIS2_PLACEMENT_3D('',#14360,#4311,#4312);
#3883=AXIS2_PLACEMENT_3D('',#14361,#4313,#4314);
#3884=AXIS2_PLACEMENT_3D('',#14363,#4315,#4316);
#3885=AXIS2_PLACEMENT_3D('',#14887,#4317,#4318);
#3886=AXIS2_PLACEMENT_3D('',#15420,#4319,#4320);
#3887=AXIS2_PLACEMENT_3D('',#15421,#4321,#4322);
#3888=AXIS2_PLACEMENT_3D('',#15423,#4323,#4324);
#3889=AXIS2_PLACEMENT_3D('',#15425,#4325,#4326);
#3890=AXIS2_PLACEMENT_3D('',#15426,#4327,#4328);
#3891=AXIS2_PLACEMENT_3D('',#15427,#4329,#4330);
#3892=AXIS2_PLACEMENT_3D('',#15430,#4332,#4333);
#3893=AXIS2_PLACEMENT_3D('',#15431,#4334,#4335);
#3894=AXIS2_PLACEMENT_3D('',#15432,#4336,#4337);
#3895=AXIS2_PLACEMENT_3D('',#15434,#4338,#4339);
#3896=AXIS2_PLACEMENT_3D('',#15436,#4340,#4341);
#3897=AXIS2_PLACEMENT_3D('',#15437,#4342,#4343);
#3898=AXIS2_PLACEMENT_3D('',#15438,#4344,#4345);
#3899=AXIS2_PLACEMENT_3D('',#15441,#4347,#4348);
#3900=AXIS2_PLACEMENT_3D('',#15442,#4349,#4350);
#3901=AXIS2_PLACEMENT_3D('',#15443,#4351,#4352);
#3902=AXIS2_PLACEMENT_3D('',#15445,#4353,#4354);
#3903=AXIS2_PLACEMENT_3D('',#15446,#4355,#4356);
#3904=AXIS2_PLACEMENT_3D('',#15447,#4357,#4358);
#3905=AXIS2_PLACEMENT_3D('',#15449,#4359,#4360);
#3906=AXIS2_PLACEMENT_3D('',#15450,#4361,#4362);
#3907=AXIS2_PLACEMENT_3D('',#15452,#4363,#4364);
#3908=AXIS2_PLACEMENT_3D('',#15454,#4365,#4366);
#3909=AXIS2_PLACEMENT_3D('',#15455,#4367,#4368);
#3910=AXIS2_PLACEMENT_3D('',#15456,#4369,#4370);
#3911=AXIS2_PLACEMENT_3D('',#15459,#4372,#4373);
#3912=AXIS2_PLACEMENT_3D('',#15460,#4374,#4375);
#3913=AXIS2_PLACEMENT_3D('',#15462,#4376,#4377);
#3914=AXIS2_PLACEMENT_3D('',#15463,#4378,#4379);
#3915=AXIS2_PLACEMENT_3D('',#15464,#4380,#4381);
#3916=AXIS2_PLACEMENT_3D('',#15465,#4382,#4383);
#3917=AXIS2_PLACEMENT_3D('',#15467,#4384,#4385);
#3918=AXIS2_PLACEMENT_3D('',#15468,#4386,#4387);
#3919=AXIS2_PLACEMENT_3D('',#15469,#4388,#4389);
#3920=AXIS2_PLACEMENT_3D('',#15472,#4391,#4392);
#3921=AXIS2_PLACEMENT_3D('',#15473,#4393,#4394);
#3922=AXIS2_PLACEMENT_3D('',#15475,#4395,#4396);
#3923=AXIS2_PLACEMENT_3D('',#15476,#4397,#4398);
#3924=AXIS2_PLACEMENT_3D('',#15477,#4399,#4400);
#3925=AXIS2_PLACEMENT_3D('',#15479,#4401,#4402);
#3926=AXIS2_PLACEMENT_3D('',#15480,#4403,#4404);
#3927=AXIS2_PLACEMENT_3D('',#15482,#4405,#4406);
#3928=AXIS2_PLACEMENT_3D('',#15484,#4407,#4408);
#3929=AXIS2_PLACEMENT_3D('',#15485,#4409,#4410);
#3930=AXIS2_PLACEMENT_3D('',#15486,#4411,#4412);
#3931=AXIS2_PLACEMENT_3D('',#15489,#4414,#4415);
#3932=AXIS2_PLACEMENT_3D('',#15490,#4416,#4417);
#3933=AXIS2_PLACEMENT_3D('',#15492,#4418,#4419);
#3934=AXIS2_PLACEMENT_3D('',#15493,#4420,#4421);
#3935=AXIS2_PLACEMENT_3D('',#15495,#4422,#4423);
#3936=AXIS2_PLACEMENT_3D('',#15496,#4424,#4425);
#3937=AXIS2_PLACEMENT_3D('',#15497,#4426,#4427);
#3938=AXIS2_PLACEMENT_3D('',#15499,#4428,#4429);
#3939=AXIS2_PLACEMENT_3D('',#15500,#4430,#4431);
#3940=AXIS2_PLACEMENT_3D('',#15502,#4432,#4433);
#3941=AXIS2_PLACEMENT_3D('',#15504,#4434,#4435);
#3942=AXIS2_PLACEMENT_3D('',#15505,#4436,#4437);
#3943=AXIS2_PLACEMENT_3D('',#15506,#4438,#4439);
#3944=AXIS2_PLACEMENT_3D('',#15507,#4440,#4441);
#3945=AXIS2_PLACEMENT_3D('',#15509,#4443,#4444);
#3946=AXIS2_PLACEMENT_3D('',#15511,#4446,#4447);
#3947=AXIS2_PLACEMENT_3D('',#15513,#4449,#4450);
#3948=AXIS2_PLACEMENT_3D('',#15576,#4453,#4454);
#3949=AXIS2_PLACEMENT_3D('',#15578,#4455,#4456);
#3950=AXIS2_PLACEMENT_3D('',#15580,#4457,#4458);
#3951=AXIS2_PLACEMENT_3D('',#15641,#4461,#4462);
#3952=AXIS2_PLACEMENT_3D('',#15642,#4463,#4464);
#3953=AXIS2_PLACEMENT_3D('',#15643,#4465,#4466);
#3954=AXIS2_PLACEMENT_3D('',#15644,#4467,#4468);
#3955=AXIS2_PLACEMENT_3D('',#15653,#4473,#4474);
#3956=AXIS2_PLACEMENT_3D('',#15659,#4478,#4479);
#3957=AXIS2_PLACEMENT_3D('',#15665,#4483,#4484);
#3958=AXIS2_PLACEMENT_3D('',#15671,#4488,#4489);
#3959=AXIS2_PLACEMENT_3D('',#15677,#4493,#4494);
#3960=AXIS2_PLACEMENT_3D('',#15680,#4497,#4498);
#3961=AXIS2_PLACEMENT_3D('',#15681,#4499,#4500);
#3962=AXIS2_PLACEMENT_3D('',#15682,#4501,#4502);
#3963=AXIS2_PLACEMENT_3D('',#15683,#4503,#4504);
#3964=AXIS2_PLACEMENT_3D('',#15843,#4506,#4507);
#3965=AXIS2_PLACEMENT_3D('',#15956,#4508,#4509);
#3966=AXIS2_PLACEMENT_3D('',#16349,#4511,#4512);
#3967=AXIS2_PLACEMENT_3D('',#16708,#4514,#4515);
#3968=AXIS2_PLACEMENT_3D('',#17049,#4517,#4518);
#3969=AXIS2_PLACEMENT_3D('',#17392,#4520,#4521);
#3970=AXIS2_PLACEMENT_3D('',#17780,#4523,#4524);
#3971=AXIS2_PLACEMENT_3D('',#17860,#4525,#4526);
#3972=AXIS2_PLACEMENT_3D('',#19120,#4527,#4528);
#3973=AXIS2_PLACEMENT_3D('',#20520,#4529,#4530);
#3974=AXIS2_PLACEMENT_3D('',#20712,#4531,#4532);
#3975=AXIS2_PLACEMENT_3D('',#21087,#4533,#4534);
#3976=AXIS2_PLACEMENT_3D('',#21089,#4535,#4536);
#3977=AXIS2_PLACEMENT_3D('',#21091,#4537,#4538);
#3978=AXIS2_PLACEMENT_3D('',#21320,#4539,#4540);
#3979=AXIS2_PLACEMENT_3D('',#21322,#4541,#4542);
#3980=AXIS2_PLACEMENT_3D('',#21323,#4543,#4544);
#3981=AXIS2_PLACEMENT_3D('',#21324,#4545,#4546);
#3982=AXIS2_PLACEMENT_3D('',#21326,#4547,#4548);
#3983=AXIS2_PLACEMENT_3D('',#21328,#4550,#4551);
#3984=AXIS2_PLACEMENT_3D('',#22110,#4552,#4553);
#3985=AXIS2_PLACEMENT_3D('',#22112,#4554,#4555);
#3986=AXIS2_PLACEMENT_3D('',#22115,#4557,#4558);
#3987=AXIS2_PLACEMENT_3D('',#22116,#4559,#4560);
#3988=AXIS2_PLACEMENT_3D('',#22117,#4561,#4562);
#3989=AXIS2_PLACEMENT_3D('',#22118,#4563,#4564);
#3990=AXIS2_PLACEMENT_3D('',#22119,#4565,#4566);
#3991=AXIS2_PLACEMENT_3D('',#22120,#4567,#4568);
#3992=AXIS2_PLACEMENT_3D('',#22122,#4569,#4570);
#3993=AXIS2_PLACEMENT_3D('',#22124,#4571,#4572);
#3994=AXIS2_PLACEMENT_3D('',#22125,#4573,#4574);
#3995=AXIS2_PLACEMENT_3D('',#22126,#4575,#4576);
#3996=AXIS2_PLACEMENT_3D('',#22129,#4578,#4579);
#3997=AXIS2_PLACEMENT_3D('',#22130,#4580,#4581);
#3998=AXIS2_PLACEMENT_3D('',#22131,#4582,#4583);
#3999=AXIS2_PLACEMENT_3D('',#22133,#4584,#4585);
#4000=AXIS2_PLACEMENT_3D('',#22134,#4586,#4587);
#4001=AXIS2_PLACEMENT_3D('',#22135,#4588,#4589);
#4002=AXIS2_PLACEMENT_3D('',#22136,#4590,#4591);
#4003=AXIS2_PLACEMENT_3D('',#22137,#4592,#4593);
#4004=AXIS2_PLACEMENT_3D('',#22139,#4594,#4595);
#4005=AXIS2_PLACEMENT_3D('',#22141,#4596,#4597);
#4006=AXIS2_PLACEMENT_3D('',#22142,#4598,#4599);
#4007=AXIS2_PLACEMENT_3D('',#22143,#4600,#4601);
#4008=AXIS2_PLACEMENT_3D('',#22146,#4603,#4604);
#4009=AXIS2_PLACEMENT_3D('',#22147,#4605,#4606);
#4010=AXIS2_PLACEMENT_3D('',#22148,#4607,#4608);
#4011=AXIS2_PLACEMENT_3D('',#22150,#4609,#4610);
#4012=AXIS2_PLACEMENT_3D('',#22151,#4611,#4612);
#4013=AXIS2_PLACEMENT_3D('',#22152,#4613,#4614);
#4014=AXIS2_PLACEMENT_3D('',#22153,#4615,#4616);
#4015=AXIS2_PLACEMENT_3D('',#22154,#4617,#4618);
#4016=AXIS2_PLACEMENT_3D('',#22450,#4647,#4648);
#4017=AXIS2_PLACEMENT_3D('',#22746,#4677,#4678);
#4018=AXIS2_PLACEMENT_3D('',#22785,#4679,#4680);
#4019=AXIS2_PLACEMENT_3D('',#22786,#4681,#4682);
#4020=AXIS2_PLACEMENT_3D('',#22933,#4683,#4684);
#4021=AXIS2_PLACEMENT_3D('',#23080,#4685,#4686);
#4022=AXIS2_PLACEMENT_3D('',#23227,#4687,#4688);
#4023=AXIS2_PLACEMENT_3D('',#23374,#4689,#4690);
#4024=AXIS2_PLACEMENT_3D('',#23521,#4691,#4692);
#4025=AXIS2_PLACEMENT_3D('',#23668,#4693,#4694);
#4026=AXIS2_PLACEMENT_3D('',#23815,#4695,#4696);
#4027=AXIS2_PLACEMENT_3D('',#23962,#4697,#4698);
#4028=AXIS2_PLACEMENT_3D('',#24109,#4699,#4700);
#4029=AXIS2_PLACEMENT_3D('',#24256,#4701,#4702);
#4030=AXIS2_PLACEMENT_3D('',#24403,#4703,#4704);
#4031=AXIS2_PLACEMENT_3D('',#24550,#4705,#4706);
#4032=AXIS2_PLACEMENT_3D('',#24611,#4707,#4708);
#4033=AXIS2_PLACEMENT_3D('',#24639,#4709,#4710);
#4034=AXIS2_PLACEMENT_3D('',#24951,#4711,#4712);
#4035=AXIS2_PLACEMENT_3D('',#25132,#4713,#4714);
#4036=AXIS2_PLACEMENT_3D('',#25176,#4715,#4716);
#4037=AXIS2_PLACEMENT_3D('',#25177,#4717,#4718);
#4038=AXIS2_PLACEMENT_3D('',#25178,#4719,#4720);
#4039=AXIS2_PLACEMENT_3D('',#25186,#4721,#4722);
#4040=AXIS2_PLACEMENT_3D('',#25187,#4723,#4724);
#4041=AXIS2_PLACEMENT_3D('',#25246,#4725,#4726);
#4042=AXIS2_PLACEMENT_3D('',#25253,#4727,#4728);
#4043=AXIS2_PLACEMENT_3D('',#25260,#4729,#4730);
#4044=AXIS2_PLACEMENT_3D('',#25267,#4731,#4732);
#4045=AXIS2_PLACEMENT_3D('',#25274,#4733,#4734);
#4046=AXIS2_PLACEMENT_3D('',#25281,#4735,#4736);
#4047=AXIS2_PLACEMENT_3D('',#25288,#4737,#4738);
#4048=AXIS2_PLACEMENT_3D('',#25295,#4739,#4740);
#4049=AXIS2_PLACEMENT_3D('',#25302,#4741,#4742);
#4050=AXIS2_PLACEMENT_3D('',#25309,#4743,#4744);
#4051=AXIS2_PLACEMENT_3D('',#25316,#4745,#4746);
#4052=AXIS2_PLACEMENT_3D('',#25635,#4747,#4748);
#4053=AXIS2_PLACEMENT_3D('',#25652,#4749,#4750);
#4054=AXIS2_PLACEMENT_3D('',#25653,#4751,#4752);
#4055=AXIS2_PLACEMENT_3D('',#25655,#4753,#4754);
#4056=AXIS2_PLACEMENT_3D('',#25658,#4756,#4757);
#4057=AXIS2_PLACEMENT_3D('',#25659,#4758,#4759);
#4058=AXIS2_PLACEMENT_3D('',#25660,#4760,#4761);
#4059=AXIS2_PLACEMENT_3D('',#25661,#4762,#4763);
#4060=AXIS2_PLACEMENT_3D('',#25662,#4764,#4765);
#4061=AXIS2_PLACEMENT_3D('',#25664,#4766,#4767);
#4062=AXIS2_PLACEMENT_3D('',#25667,#4769,#4770);
#4063=AXIS2_PLACEMENT_3D('',#25668,#4771,#4772);
#4064=AXIS2_PLACEMENT_3D('',#25670,#4773,#4774);
#4065=AXIS2_PLACEMENT_3D('',#25671,#4775,#4776);
#4066=AXIS2_PLACEMENT_3D('',#25672,#4777,#4778);
#4067=AXIS2_PLACEMENT_3D('',#25673,#4779,#4780);
#4068=AXIS2_PLACEMENT_3D('',#25675,#4781,#4782);
#4069=AXIS2_PLACEMENT_3D('',#25677,#4783,#4784);
#4070=AXIS2_PLACEMENT_3D('',#25678,#4785,#4786);
#4071=AXIS2_PLACEMENT_3D('',#25679,#4787,#4788);
#4072=AXIS2_PLACEMENT_3D('',#25681,#4789,#4790);
#4073=AXIS2_PLACEMENT_3D('',#25682,#4791,#4792);
#4074=AXIS2_PLACEMENT_3D('',#25684,#4794,#4795);
#4075=AXIS2_PLACEMENT_3D('',#25686,#4796,#4797);
#4076=AXIS2_PLACEMENT_3D('',#25689,#4799,#4800);
#4077=AXIS2_PLACEMENT_3D('',#25690,#4801,#4802);
#4078=AXIS2_PLACEMENT_3D('',#25692,#4803,#4804);
#4079=AXIS2_PLACEMENT_3D('',#25695,#4806,#4807);
#4080=AXIS2_PLACEMENT_3D('',#25696,#4808,#4809);
#4081=AXIS2_PLACEMENT_3D('',#25697,#4810,#4811);
#4082=AXIS2_PLACEMENT_3D('',#25699,#4812,#4813);
#4083=AXIS2_PLACEMENT_3D('',#25701,#4815,#4816);
#4084=AXIS2_PLACEMENT_3D('',#25704,#4818,#4819);
#4085=AXIS2_PLACEMENT_3D('',#25705,#4820,#4821);
#4086=AXIS2_PLACEMENT_3D('',#25706,#4822,#4823);
#4087=AXIS2_PLACEMENT_3D('',#25769,#4826,#4827);
#4088=AXIS2_PLACEMENT_3D('',#25771,#4828,#4829);
#4089=AXIS2_PLACEMENT_3D('',#25773,#4830,#4831);
#4090=AXIS2_PLACEMENT_3D('',#25834,#4834,#4835);
#4091=AXIS2_PLACEMENT_3D('',#25835,#4836,#4837);
#4092=AXIS2_PLACEMENT_3D('',#25836,#4838,#4839);
#4093=AXIS2_PLACEMENT_3D('',#25837,#4840,#4841);
#4094=AXIS2_PLACEMENT_3D('',#25846,#4846,#4847);
#4095=AXIS2_PLACEMENT_3D('',#25852,#4851,#4852);
#4096=AXIS2_PLACEMENT_3D('',#25858,#4856,#4857);
#4097=AXIS2_PLACEMENT_3D('',#25864,#4861,#4862);
#4098=AXIS2_PLACEMENT_3D('',#25870,#4866,#4867);
#4099=AXIS2_PLACEMENT_3D('',#25873,#4870,#4871);
#4100=AXIS2_PLACEMENT_3D('',#25874,#4872,#4873);
#4101=AXIS2_PLACEMENT_3D('',#25875,#4874,#4875);
#4102=AXIS2_PLACEMENT_3D('',#28020,#4876,#4877);
#4103=AXIS2_PLACEMENT_3D('',#28021,#4878,#4879);
#4104=AXIS2_PLACEMENT_3D('',#28022,#4880,#4881);
#4105=AXIS2_PLACEMENT_3D('',#28023,#4882,#4883);
#4106=AXIS2_PLACEMENT_3D('',#28024,#4884,#4885);
#4107=AXIS2_PLACEMENT_3D('',#28025,#4886,#4887);
#4108=AXIS2_PLACEMENT_3D('',#28026,#4888,#4889);
#4109=AXIS2_PLACEMENT_3D('',#28027,#4890,#4891);
#4110=AXIS2_PLACEMENT_3D('',#28028,#4892,#4893);
#4111=AXIS2_PLACEMENT_3D('',#28029,#4894,#4895);
#4112=AXIS2_PLACEMENT_3D('',#28030,#4896,#4897);
#4113=AXIS2_PLACEMENT_3D('',#28031,#4898,#4899);
#4114=DIRECTION('axis',(0.,0.,1.));
#4115=DIRECTION('refdir',(1.,0.,0.));
#4116=DIRECTION('axis',(0.,0.,1.));
#4117=DIRECTION('refdir',(1.,0.,0.));
#4118=DIRECTION('center_axis',(0.,1.,0.));
#4119=DIRECTION('ref_axis',(1.,0.,0.));
#4120=DIRECTION('',(0.,1.,0.));
#4121=DIRECTION('center_axis',(1.,0.,0.));
#4122=DIRECTION('ref_axis',(0.,-1.,0.));
#4123=DIRECTION('center_axis',(1.,0.,0.));
#4124=DIRECTION('ref_axis',(0.,-1.,0.));
#4125=DIRECTION('',(1.,0.,0.));
#4126=DIRECTION('center_axis',(1.,0.,0.));
#4127=DIRECTION('ref_axis',(0.,-1.,0.));
#4128=DIRECTION('center_axis',(-1.,0.,0.));
#4129=DIRECTION('ref_axis',(0.,-1.,0.));
#4130=DIRECTION('center_axis',(1.,0.,0.));
#4131=DIRECTION('ref_axis',(0.,0.,-1.));
#4132=DIRECTION('center_axis',(1.,0.,0.));
#4133=DIRECTION('ref_axis',(0.,0.,-1.));
#4134=DIRECTION('center_axis',(1.,0.,0.));
#4135=DIRECTION('ref_axis',(0.,0.,-1.));
#4136=DIRECTION('',(-0.819194986126072,7.02353436578877E-17,-0.573515104165448));
#4137=DIRECTION('center_axis',(1.,0.,0.));
#4138=DIRECTION('ref_axis',(0.,0.,-1.));
#4139=DIRECTION('center_axis',(1.,0.,0.));
#4140=DIRECTION('ref_axis',(0.,0.,-1.));
#4141=DIRECTION('center_axis',(1.,0.,0.));
#4142=DIRECTION('ref_axis',(0.,0.,-1.));
#4143=DIRECTION('',(-1.,0.,0.));
#4144=DIRECTION('center_axis',(-1.,0.,0.));
#4145=DIRECTION('ref_axis',(0.,0.,-1.));
#4146=DIRECTION('',(0.848733460294827,-6.47618786727041E-17,-0.528820870783264));
#4147=DIRECTION('center_axis',(1.,0.,0.));
#4148=DIRECTION('ref_axis',(0.,0.,-1.));
#4149=DIRECTION('center_axis',(1.,0.,0.));
#4150=DIRECTION('ref_axis',(0.,0.,-1.));
#4151=DIRECTION('center_axis',(1.,0.,0.));
#4152=DIRECTION('ref_axis',(0.,0.,-1.));
#4153=DIRECTION('',(-0.819194986126072,7.02353436578877E-17,-0.573515104165448));
#4154=DIRECTION('center_axis',(1.,0.,0.));
#4155=DIRECTION('ref_axis',(0.,0.,-1.));
#4156=DIRECTION('center_axis',(1.,0.,0.));
#4157=DIRECTION('ref_axis',(0.,0.,-1.));
#4158=DIRECTION('',(-1.,0.,0.));
#4159=DIRECTION('center_axis',(-1.,0.,0.));
#4160=DIRECTION('ref_axis',(0.,0.,-1.));
#4161=DIRECTION('',(0.790828861928077,-7.49529574979538E-17,-0.612037344564482));
#4162=DIRECTION('center_axis',(1.,0.,0.));
#4163=DIRECTION('ref_axis',(0.,0.,-1.));
#4164=DIRECTION('center_axis',(1.,0.,0.));
#4165=DIRECTION('ref_axis',(0.,0.,-1.));
#4166=DIRECTION('center_axis',(1.,0.,0.));
#4167=DIRECTION('ref_axis',(0.,0.,-1.));
#4168=DIRECTION('',(0.999999956307574,-3.62016965809164E-20,0.00029560928592735));
#4169=DIRECTION('center_axis',(1.,0.,0.));
#4170=DIRECTION('ref_axis',(0.,0.,-1.));
#4171=DIRECTION('center_axis',(1.,0.,0.));
#4172=DIRECTION('ref_axis',(0.,0.,-1.));
#4173=DIRECTION('',(1.,0.,0.));
#4174=DIRECTION('center_axis',(1.,0.,0.));
#4175=DIRECTION('ref_axis',(0.,0.,-1.));
#4176=DIRECTION('center_axis',(1.,0.,0.));
#4177=DIRECTION('ref_axis',(0.,0.,-1.));
#4178=DIRECTION('',(0.999999956307574,-3.62016965809512E-20,0.000295609285927634));
#4179=DIRECTION('center_axis',(-1.,0.,0.));
#4180=DIRECTION('ref_axis',(0.,0.,1.));
#4181=DIRECTION('center_axis',(1.,0.,0.));
#4182=DIRECTION('ref_axis',(0.,0.,-1.));
#4183=DIRECTION('center_axis',(1.,0.,0.));
#4184=DIRECTION('ref_axis',(0.,0.,-1.));
#4185=DIRECTION('center_axis',(1.,0.,0.));
#4186=DIRECTION('ref_axis',(0.,0.,-1.));
#4187=DIRECTION('',(1.,0.,0.));
#4188=DIRECTION('center_axis',(1.,0.,0.));
#4189=DIRECTION('ref_axis',(0.,0.,-1.));
#4190=DIRECTION('center_axis',(1.,0.,0.));
#4191=DIRECTION('ref_axis',(0.,0.,-1.));
#4192=DIRECTION('center_axis',(1.,0.,0.));
#4193=DIRECTION('ref_axis',(0.,0.,-1.));
#4194=DIRECTION('center_axis',(1.,0.,0.));
#4195=DIRECTION('ref_axis',(0.,0.,-1.));
#4196=DIRECTION('',(0.999999956307574,-3.62016965809699E-20,0.000295609285927787));
#4197=DIRECTION('center_axis',(1.,0.,0.));
#4198=DIRECTION('ref_axis',(0.,0.,-1.));
#4199=DIRECTION('center_axis',(1.,0.,0.));
#4200=DIRECTION('ref_axis',(0.,0.,-1.));
#4201=DIRECTION('',(1.,0.,0.));
#4202=DIRECTION('center_axis',(1.,0.,0.));
#4203=DIRECTION('ref_axis',(0.,0.,-1.));
#4204=DIRECTION('center_axis',(1.,0.,0.));
#4205=DIRECTION('ref_axis',(0.,0.,-1.));
#4206=DIRECTION('',(0.999999956307574,-3.62016965808782E-20,0.000295609285927038));
#4207=DIRECTION('center_axis',(1.,0.,0.));
#4208=DIRECTION('ref_axis',(0.,0.,-1.));
#4209=DIRECTION('center_axis',(1.,0.,0.));
#4210=DIRECTION('ref_axis',(0.,0.,-1.));
#4211=DIRECTION('',(1.,0.,0.));
#4212=DIRECTION('center_axis',(1.,0.,0.));
#4213=DIRECTION('ref_axis',(0.,0.,-1.));
#4214=DIRECTION('center_axis',(1.,0.,0.));
#4215=DIRECTION('ref_axis',(0.,0.,-1.));
#4216=DIRECTION('',(0.999999956307574,-3.62016965808193E-20,0.000295609285926557));
#4217=DIRECTION('center_axis',(1.,0.,0.));
#4218=DIRECTION('ref_axis',(0.,0.,-1.));
#4219=DIRECTION('center_axis',(1.,0.,0.));
#4220=DIRECTION('ref_axis',(0.,0.,-1.));
#4221=DIRECTION('center_axis',(1.,0.,0.));
#4222=DIRECTION('ref_axis',(0.,0.,-1.));
#4223=DIRECTION('center_axis',(1.,0.,0.));
#4224=DIRECTION('ref_axis',(0.,0.,-1.));
#4225=DIRECTION('',(1.,0.,0.));
#4226=DIRECTION('center_axis',(1.,0.,0.));
#4227=DIRECTION('ref_axis',(0.,0.,-1.));
#4228=DIRECTION('center_axis',(1.,0.,0.));
#4229=DIRECTION('ref_axis',(0.,0.,-1.));
#4230=DIRECTION('center_axis',(1.,0.,0.));
#4231=DIRECTION('ref_axis',(0.,0.,-1.));
#4232=DIRECTION('',(1.,0.,0.));
#4233=DIRECTION('center_axis',(-1.,0.,0.));
#4234=DIRECTION('ref_axis',(0.,0.,1.));
#4235=DIRECTION('axis',(0.,0.,1.));
#4236=DIRECTION('refdir',(1.,0.,0.));
#4237=DIRECTION('center_axis',(1.,0.,0.));
#4238=DIRECTION('ref_axis',(0.,-0.999641738703431,0.0267655420640338));
#4239=DIRECTION('',(-1.,0.,0.));
#4240=DIRECTION('center_axis',(-1.,0.,0.));
#4241=DIRECTION('ref_axis',(0.,9.28774802075533E-14,-1.));
#4242=DIRECTION('center_axis',(1.,0.,0.));
#4243=DIRECTION('ref_axis',(0.,-0.999641738703431,0.0267655420640338));
#4244=DIRECTION('',(-1.,0.,0.));
#4245=DIRECTION('center_axis',(1.,0.,0.));
#4246=DIRECTION('ref_axis',(0.,-0.999641738703431,0.0267655420640338));
#4247=DIRECTION('',(-1.,0.,0.));
#4248=DIRECTION('center_axis',(1.,0.,0.));
#4249=DIRECTION('ref_axis',(0.,-0.999641738703431,0.0267655420640338));
#4250=DIRECTION('',(-1.,0.,0.));
#4251=DIRECTION('center_axis',(1.,0.,0.));
#4252=DIRECTION('ref_axis',(0.,-0.999641738703431,0.0267655420640338));
#4253=DIRECTION('',(-1.,0.,0.));
#4254=DIRECTION('center_axis',(1.,0.,0.));
#4255=DIRECTION('ref_axis',(0.,-0.999641738703431,0.0267655420640338));
#4256=DIRECTION('',(-1.,0.,0.));
#4257=DIRECTION('center_axis',(1.,0.,0.));
#4258=DIRECTION('ref_axis',(0.,-0.999641738703431,0.0267655420640338));
#4259=DIRECTION('',(-1.,0.,0.));
#4260=DIRECTION('center_axis',(1.,0.,0.));
#4261=DIRECTION('ref_axis',(0.,-0.999641738703431,0.0267655420640338));
#4262=DIRECTION('',(-1.,0.,0.));
#4263=DIRECTION('center_axis',(1.,0.,0.));
#4264=DIRECTION('ref_axis',(0.,-0.999641738703431,0.0267655420640338));
#4265=DIRECTION('',(-1.,0.,0.));
#4266=DIRECTION('center_axis',(1.,0.,0.));
#4267=DIRECTION('ref_axis',(0.,-0.999641738703431,0.0267655420640338));
#4268=DIRECTION('',(-1.,0.,0.));
#4269=DIRECTION('center_axis',(1.,0.,0.));
#4270=DIRECTION('ref_axis',(0.,-0.999641738703431,0.0267655420640338));
#4271=DIRECTION('',(-1.,0.,0.));
#4272=DIRECTION('center_axis',(1.,0.,0.));
#4273=DIRECTION('ref_axis',(0.,-0.999641738703431,0.0267655420640338));
#4274=DIRECTION('',(-1.,0.,0.));
#4275=DIRECTION('center_axis',(1.,0.,0.));
#4276=DIRECTION('ref_axis',(0.,-0.999641738703431,0.0267655420640338));
#4277=DIRECTION('',(-1.,0.,0.));
#4278=DIRECTION('center_axis',(1.,0.,0.));
#4279=DIRECTION('ref_axis',(0.,0.,-1.));
#4280=DIRECTION('center_axis',(-1.,0.,0.));
#4281=DIRECTION('ref_axis',(0.,0.,-1.));
#4282=DIRECTION('center_axis',(-1.,0.,0.));
#4283=DIRECTION('ref_axis',(0.,0.,-1.));
#4284=DIRECTION('center_axis',(-1.,0.,0.));
#4285=DIRECTION('ref_axis',(0.,0.,-1.));
#4286=DIRECTION('center_axis',(1.,0.,0.));
#4287=DIRECTION('ref_axis',(0.,-0.999641738703431,0.0267655420640338));
#4288=DIRECTION('center_axis',(1.,0.,0.));
#4289=DIRECTION('ref_axis',(0.,9.28774802075533E-14,-1.));
#4290=DIRECTION('center_axis',(-1.,0.,0.));
#4291=DIRECTION('ref_axis',(0.,0.,1.));
#4292=DIRECTION('center_axis',(1.,0.,0.));
#4293=DIRECTION('ref_axis',(0.,1.22464679914735E-16,1.));
#4294=DIRECTION('center_axis',(-1.,0.,0.));
#4295=DIRECTION('ref_axis',(0.,1.22464679914735E-16,1.));
#4296=DIRECTION('center_axis',(1.,0.,0.));
#4297=DIRECTION('ref_axis',(0.,0.,-1.));
#4298=DIRECTION('center_axis',(-1.,0.,0.));
#4299=DIRECTION('ref_axis',(0.,0.,-1.));
#4300=DIRECTION('center_axis',(0.,-1.,-1.22464679914735E-16));
#4301=DIRECTION('ref_axis',(0.,-1.22464679914735E-16,1.));
#4302=DIRECTION('center_axis',(1.,0.,0.));
#4303=DIRECTION('ref_axis',(0.,0.,1.));
#4304=DIRECTION('center_axis',(1.,0.,0.));
#4305=DIRECTION('ref_axis',(0.,0.,-1.));
#4306=DIRECTION('',(-0.999999956307574,3.62016965809699E-20,-0.000295609285927787));
#4307=DIRECTION('center_axis',(-1.,0.,0.));
#4308=DIRECTION('ref_axis',(0.,0.,1.));
#4309=DIRECTION('center_axis',(1.,0.,0.));
#4310=DIRECTION('ref_axis',(0.,0.,-1.));
#4311=DIRECTION('center_axis',(0.,-1.,-1.22464679914735E-16));
#4312=DIRECTION('ref_axis',(0.,-1.22464679914735E-16,1.));
#4313=DIRECTION('center_axis',(-1.,0.,0.));
#4314=DIRECTION('ref_axis',(0.,0.,1.));
#4315=DIRECTION('center_axis',(1.,0.,0.));
#4316=DIRECTION('ref_axis',(0.,1.22464679914735E-16,1.));
#4317=DIRECTION('center_axis',(1.,0.,0.));
#4318=DIRECTION('ref_axis',(0.,0.,-1.));
#4319=DIRECTION('center_axis',(1.,0.,0.));
#4320=DIRECTION('ref_axis',(0.,0.,-1.));
#4321=DIRECTION('center_axis',(1.,0.,0.));
#4322=DIRECTION('ref_axis',(0.,0.,-1.));
#4323=DIRECTION('center_axis',(-1.,0.,0.));
#4324=DIRECTION('ref_axis',(0.,1.22464679914735E-16,1.));
#4325=DIRECTION('center_axis',(0.,-1.,-1.22464679914735E-16));
#4326=DIRECTION('ref_axis',(0.,-1.22464679914735E-16,1.));
#4327=DIRECTION('center_axis',(1.,0.,0.));
#4328=DIRECTION('ref_axis',(0.,1.22464679914735E-16,1.));
#4329=DIRECTION('center_axis',(1.,0.,0.));
#4330=DIRECTION('ref_axis',(0.,0.,-1.));
#4331=DIRECTION('',(-1.,0.,0.));
#4332=DIRECTION('center_axis',(1.,0.,0.));
#4333=DIRECTION('ref_axis',(0.,0.,-1.));
#4334=DIRECTION('center_axis',(1.,0.,0.));
#4335=DIRECTION('ref_axis',(0.,0.,-1.));
#4336=DIRECTION('center_axis',(1.,0.,0.));
#4337=DIRECTION('ref_axis',(0.,0.,-1.));
#4338=DIRECTION('center_axis',(-1.,0.,0.));
#4339=DIRECTION('ref_axis',(0.,1.22464679914735E-16,1.));
#4340=DIRECTION('center_axis',(0.,-1.,-1.22464679914735E-16));
#4341=DIRECTION('ref_axis',(0.,-1.22464679914735E-16,1.));
#4342=DIRECTION('center_axis',(1.,0.,0.));
#4343=DIRECTION('ref_axis',(0.,0.,1.));
#4344=DIRECTION('center_axis',(1.,0.,0.));
#4345=DIRECTION('ref_axis',(0.,0.,-1.));
#4346=DIRECTION('',(-0.999999956307574,3.62016965808668E-20,-0.000295609285926945));
#4347=DIRECTION('center_axis',(-1.,0.,0.));
#4348=DIRECTION('ref_axis',(0.,0.,1.));
#4349=DIRECTION('center_axis',(1.,0.,0.));
#4350=DIRECTION('ref_axis',(0.,0.,-1.));
#4351=DIRECTION('center_axis',(1.,0.,0.));
#4352=DIRECTION('ref_axis',(0.,0.,-1.));
#4353=DIRECTION('center_axis',(0.,-1.,-1.22464679914735E-16));
#4354=DIRECTION('ref_axis',(0.,-1.22464679914735E-16,1.));
#4355=DIRECTION('center_axis',(1.,0.,0.));
#4356=DIRECTION('ref_axis',(0.,1.22464679914735E-16,1.));
#4357=DIRECTION('center_axis',(-1.,0.,0.));
#4358=DIRECTION('ref_axis',(0.,0.,1.));
#4359=DIRECTION('center_axis',(1.,0.,0.));
#4360=DIRECTION('ref_axis',(0.,0.,-1.));
#4361=DIRECTION('center_axis',(1.,0.,0.));
#4362=DIRECTION('ref_axis',(0.,0.,-1.));
#4363=DIRECTION('center_axis',(-1.,0.,0.));
#4364=DIRECTION('ref_axis',(0.,1.22464679914735E-16,1.));
#4365=DIRECTION('center_axis',(0.,-1.,-1.22464679914735E-16));
#4366=DIRECTION('ref_axis',(0.,-1.22464679914735E-16,1.));
#4367=DIRECTION('center_axis',(1.,0.,0.));
#4368=DIRECTION('ref_axis',(0.,0.,1.));
#4369=DIRECTION('center_axis',(1.,0.,0.));
#4370=DIRECTION('ref_axis',(0.,0.,-1.));
#4371=DIRECTION('',(-0.999999956307574,3.62016965808707E-20,-0.000295609285926977));
#4372=DIRECTION('center_axis',(-1.,0.,0.));
#4373=DIRECTION('ref_axis',(0.,0.,1.));
#4374=DIRECTION('center_axis',(1.,0.,0.));
#4375=DIRECTION('ref_axis',(0.,0.,-1.));
#4376=DIRECTION('center_axis',(1.,0.,0.));
#4377=DIRECTION('ref_axis',(0.,0.,-1.));
#4378=DIRECTION('center_axis',(1.,0.,0.));
#4379=DIRECTION('ref_axis',(0.,0.,-1.));
#4380=DIRECTION('center_axis',(0.,-1.,-1.22464679914735E-16));
#4381=DIRECTION('ref_axis',(0.,-1.22464679914735E-16,1.));
#4382=DIRECTION('center_axis',(1.,0.,0.));
#4383=DIRECTION('ref_axis',(0.,0.,-1.));
#4384=DIRECTION('center_axis',(0.,-1.,-1.22464679914735E-16));
#4385=DIRECTION('ref_axis',(0.,-1.22464679914735E-16,1.));
#4386=DIRECTION('center_axis',(1.,0.,0.));
#4387=DIRECTION('ref_axis',(0.,0.,1.));
#4388=DIRECTION('center_axis',(1.,0.,0.));
#4389=DIRECTION('ref_axis',(0.,0.,-1.));
#4390=DIRECTION('',(-0.999999956307574,3.62016965808673E-20,-0.000295609285926949));
#4391=DIRECTION('center_axis',(-1.,0.,0.));
#4392=DIRECTION('ref_axis',(0.,0.,1.));
#4393=DIRECTION('center_axis',(1.,0.,0.));
#4394=DIRECTION('ref_axis',(0.,0.,-1.));
#4395=DIRECTION('center_axis',(0.,-1.,-1.22464679914735E-16));
#4396=DIRECTION('ref_axis',(0.,-1.22464679914735E-16,1.));
#4397=DIRECTION('center_axis',(1.,0.,0.));
#4398=DIRECTION('ref_axis',(0.,1.22464679914735E-16,1.));
#4399=DIRECTION('center_axis',(-1.,0.,0.));
#4400=DIRECTION('ref_axis',(0.,0.,1.));
#4401=DIRECTION('center_axis',(1.,0.,0.));
#4402=DIRECTION('ref_axis',(0.,0.,-1.));
#4403=DIRECTION('center_axis',(1.,0.,0.));
#4404=DIRECTION('ref_axis',(0.,0.,-1.));
#4405=DIRECTION('center_axis',(-1.,0.,0.));
#4406=DIRECTION('ref_axis',(0.,1.22464679914735E-16,1.));
#4407=DIRECTION('center_axis',(0.,-1.,-1.22464679914735E-16));
#4408=DIRECTION('ref_axis',(0.,-1.22464679914735E-16,1.));
#4409=DIRECTION('center_axis',(1.,0.,0.));
#4410=DIRECTION('ref_axis',(0.,0.,1.));
#4411=DIRECTION('center_axis',(1.,0.,0.));
#4412=DIRECTION('ref_axis',(0.,0.,-1.));
#4413=DIRECTION('',(-0.999999956307574,3.62016965810123E-20,-0.000295609285928133));
#4414=DIRECTION('center_axis',(-1.,0.,0.));
#4415=DIRECTION('ref_axis',(0.,0.,1.));
#4416=DIRECTION('center_axis',(1.,0.,0.));
#4417=DIRECTION('ref_axis',(0.,0.,-1.));
#4418=DIRECTION('center_axis',(1.,0.,0.));
#4419=DIRECTION('ref_axis',(0.,0.,-1.));
#4420=DIRECTION('center_axis',(1.,0.,0.));
#4421=DIRECTION('ref_axis',(0.,0.,-1.));
#4422=DIRECTION('center_axis',(0.,-1.,-1.22464679914735E-16));
#4423=DIRECTION('ref_axis',(0.,-1.22464679914735E-16,1.));
#4424=DIRECTION('center_axis',(1.,0.,0.));
#4425=DIRECTION('ref_axis',(0.,1.22464679914735E-16,1.));
#4426=DIRECTION('center_axis',(-1.,0.,0.));
#4427=DIRECTION('ref_axis',(0.,0.,1.));
#4428=DIRECTION('center_axis',(1.,0.,0.));
#4429=DIRECTION('ref_axis',(0.,0.,-1.));
#4430=DIRECTION('center_axis',(1.,0.,0.));
#4431=DIRECTION('ref_axis',(0.,0.,-1.));
#4432=DIRECTION('center_axis',(-1.,0.,0.));
#4433=DIRECTION('ref_axis',(0.,1.22464679914735E-16,1.));
#4434=DIRECTION('center_axis',(0.,-1.,-1.22464679914735E-16));
#4435=DIRECTION('ref_axis',(0.,-1.22464679914735E-16,1.));
#4436=DIRECTION('center_axis',(1.,0.,0.));
#4437=DIRECTION('ref_axis',(0.,1.22464679914735E-16,1.));
#4438=DIRECTION('center_axis',(-1.,0.,0.));
#4439=DIRECTION('ref_axis',(0.,0.,1.));
#4440=DIRECTION('center_axis',(1.,0.,0.));
#4441=DIRECTION('ref_axis',(0.,0.,-1.));
#4442=DIRECTION('',(-1.,0.,0.));
#4443=DIRECTION('center_axis',(1.,0.,0.));
#4444=DIRECTION('ref_axis',(0.,0.,-1.));
#4445=DIRECTION('',(-1.,0.,0.));
#4446=DIRECTION('center_axis',(1.,0.,0.));
#4447=DIRECTION('ref_axis',(0.,0.,-1.));
#4448=DIRECTION('',(-1.,0.,0.));
#4449=DIRECTION('axis',(0.,0.,1.));
#4450=DIRECTION('refdir',(1.,0.,0.));
#4451=DIRECTION('',(1.,0.,0.));
#4452=DIRECTION('',(1.,0.,0.));
#4453=DIRECTION('center_axis',(1.,0.,0.));
#4454=DIRECTION('ref_axis',(0.,0.444750988585694,0.895654262621492));
#4455=DIRECTION('center_axis',(-1.,0.,0.));
#4456=DIRECTION('ref_axis',(0.,0.444750988585694,0.895654262621492));
#4457=DIRECTION('center_axis',(-1.,0.,0.));
#4458=DIRECTION('ref_axis',(0.,0.444750988585694,0.895654262621492));
#4459=DIRECTION('',(1.,0.,0.));
#4460=DIRECTION('',(1.,0.,0.));
#4461=DIRECTION('center_axis',(1.,0.,0.));
#4462=DIRECTION('ref_axis',(0.,-0.580623944517215,-0.814171870708679));
#4463=DIRECTION('center_axis',(-1.,0.,0.));
#4464=DIRECTION('ref_axis',(0.,-0.580623944517215,-0.814171870708679));
#4465=DIRECTION('center_axis',(-1.,0.,0.));
#4466=DIRECTION('ref_axis',(0.,-0.580623944517215,-0.814171870708679));
#4467=DIRECTION('center_axis',(0.,0.866025403784439,0.5));
#4468=DIRECTION('ref_axis',(0.,-0.5,0.866025403784439));
#4469=DIRECTION('',(0.,-0.5,0.866025403784439));
#4470=DIRECTION('',(1.,0.,0.));
#4471=DIRECTION('',(0.,-0.5,0.866025403784439));
#4472=DIRECTION('',(1.,0.,0.));
#4473=DIRECTION('center_axis',(0.,0.866025403784438,-0.5));
#4474=DIRECTION('ref_axis',(0.,0.5,0.866025403784438));
#4475=DIRECTION('',(0.,0.5,0.866025403784438));
#4476=DIRECTION('',(0.,0.5,0.866025403784438));
#4477=DIRECTION('',(1.,0.,0.));
#4478=DIRECTION('center_axis',(0.,-3.02823770847138E-16,-1.));
#4479=DIRECTION('ref_axis',(0.,1.,-3.02823770847138E-16));
#4480=DIRECTION('',(0.,1.,-3.02823770847138E-16));
#4481=DIRECTION('',(0.,1.,-3.02823770847138E-16));
#4482=DIRECTION('',(1.,0.,0.));
#4483=DIRECTION('center_axis',(0.,-0.866025403784439,-0.5));
#4484=DIRECTION('ref_axis',(0.,0.5,-0.866025403784439));
#4485=DIRECTION('',(0.,0.5,-0.866025403784439));
#4486=DIRECTION('',(0.,0.5,-0.866025403784439));
#4487=DIRECTION('',(1.,0.,0.));
#4488=DIRECTION('center_axis',(0.,-0.866025403784439,0.5));
#4489=DIRECTION('ref_axis',(0.,-0.5,-0.866025403784439));
#4490=DIRECTION('',(0.,-0.5,-0.866025403784439));
#4491=DIRECTION('',(0.,-0.5,-0.866025403784439));
#4492=DIRECTION('',(1.,0.,0.));
#4493=DIRECTION('center_axis',(0.,6.05647541694275E-16,1.));
#4494=DIRECTION('ref_axis',(0.,-1.,6.05647541694275E-16));
#4495=DIRECTION('',(0.,-1.,6.05647541694275E-16));
#4496=DIRECTION('',(0.,-1.,6.05647541694275E-16));
#4497=DIRECTION('center_axis',(1.,0.,0.));
#4498=DIRECTION('ref_axis',(0.,1.,0.));
#4499=DIRECTION('center_axis',(1.,0.,0.));
#4500=DIRECTION('ref_axis',(0.,1.,0.));
#4501=DIRECTION('axis',(0.,0.,1.));
#4502=DIRECTION('refdir',(1.,0.,0.));
#4503=DIRECTION('center_axis',(1.,0.,0.));
#4504=DIRECTION('ref_axis',(0.,0.704081661975572,-0.710119013454587));
#4505=DIRECTION('',(-1.,0.,0.));
#4506=DIRECTION('center_axis',(-1.,0.,0.));
#4507=DIRECTION('ref_axis',(0.,1.,2.1444273868172E-14));
#4508=DIRECTION('center_axis',(1.,0.,0.));
#4509=DIRECTION('ref_axis',(0.,0.704081661975572,-0.710119013454587));
#4510=DIRECTION('',(-1.,0.,0.));
#4511=DIRECTION('center_axis',(1.,0.,0.));
#4512=DIRECTION('ref_axis',(0.,0.704081661975572,-0.710119013454587));
#4513=DIRECTION('',(-1.,0.,0.));
#4514=DIRECTION('center_axis',(1.,0.,0.));
#4515=DIRECTION('ref_axis',(0.,0.704081661975572,-0.710119013454587));
#4516=DIRECTION('',(-1.,0.,0.));
#4517=DIRECTION('center_axis',(1.,0.,0.));
#4518=DIRECTION('ref_axis',(0.,0.704081661975572,-0.710119013454587));
#4519=DIRECTION('',(-1.,0.,0.));
#4520=DIRECTION('center_axis',(1.,0.,0.));
#4521=DIRECTION('ref_axis',(0.,0.704081661975572,-0.710119013454587));
#4522=DIRECTION('',(-1.,0.,0.));
#4523=DIRECTION('center_axis',(1.,0.,0.));
#4524=DIRECTION('ref_axis',(0.,1.,0.));
#4525=DIRECTION('center_axis',(-1.,0.,0.));
#4526=DIRECTION('ref_axis',(0.,1.,0.));
#4527=DIRECTION('center_axis',(-1.,0.,0.));
#4528=DIRECTION('ref_axis',(0.,1.,0.));
#4529=DIRECTION('center_axis',(1.,0.,0.));
#4530=DIRECTION('ref_axis',(0.,0.704081661975572,-0.710119013454587));
#4531=DIRECTION('center_axis',(1.,0.,0.));
#4532=DIRECTION('ref_axis',(0.,1.,2.1444273868172E-14));
#4533=DIRECTION('center_axis',(1.,0.,0.));
#4534=DIRECTION('ref_axis',(0.,-0.692346234554118,0.72156544505591));
#4535=DIRECTION('center_axis',(-1.,0.,0.));
#4536=DIRECTION('ref_axis',(0.,9.28774802075533E-14,-1.));
#4537=DIRECTION('center_axis',(-1.,0.,0.));
#4538=DIRECTION('ref_axis',(0.,9.28774802075533E-14,-1.));
#4539=DIRECTION('center_axis',(1.,0.,0.));
#4540=DIRECTION('ref_axis',(0.,0.,-1.));
#4541=DIRECTION('center_axis',(-1.,0.,0.));
#4542=DIRECTION('ref_axis',(0.,0.,-1.));
#4543=DIRECTION('center_axis',(-1.,0.,0.));
#4544=DIRECTION('ref_axis',(0.,0.,-1.));
#4545=DIRECTION('center_axis',(1.,0.,0.));
#4546=DIRECTION('ref_axis',(0.,0.,-1.));
#4547=DIRECTION('center_axis',(1.,0.,0.));
#4548=DIRECTION('ref_axis',(0.,0.,-1.));
#4549=DIRECTION('',(1.,0.,0.));
#4550=DIRECTION('center_axis',(-1.,0.,0.));
#4551=DIRECTION('ref_axis',(0.,0.,-1.));
#4552=DIRECTION('center_axis',(1.,0.,0.));
#4553=DIRECTION('ref_axis',(0.,1.,0.));
#4554=DIRECTION('center_axis',(1.,0.,0.));
#4555=DIRECTION('ref_axis',(0.,1.,0.));
#4556=DIRECTION('',(-1.,0.,0.));
#4557=DIRECTION('center_axis',(1.,0.,0.));
#4558=DIRECTION('ref_axis',(0.,1.,0.));
#4559=DIRECTION('center_axis',(1.,0.,0.));
#4560=DIRECTION('ref_axis',(0.,1.,0.));
#4561=DIRECTION('center_axis',(1.,0.,0.));
#4562=DIRECTION('ref_axis',(0.,1.,0.));
#4563=DIRECTION('center_axis',(1.,0.,0.));
#4564=DIRECTION('ref_axis',(0.,1.,0.));
#4565=DIRECTION('axis',(0.,0.,1.));
#4566=DIRECTION('refdir',(1.,0.,0.));
#4567=DIRECTION('center_axis',(1.,0.,0.));
#4568=DIRECTION('ref_axis',(0.,0.,-1.));
#4569=DIRECTION('center_axis',(-1.,0.,0.));
#4570=DIRECTION('ref_axis',(0.,1.22464679914735E-16,1.));
#4571=DIRECTION('center_axis',(0.,-1.,-1.22464679914735E-16));
#4572=DIRECTION('ref_axis',(0.,-1.22464679914735E-16,1.));
#4573=DIRECTION('center_axis',(1.,0.,0.));
#4574=DIRECTION('ref_axis',(0.,0.,1.));
#4575=DIRECTION('center_axis',(1.,0.,0.));
#4576=DIRECTION('ref_axis',(0.,0.,-1.));
#4577=DIRECTION('',(-0.999999956307574,3.62016965809512E-20,-0.000295609285927634));
#4578=DIRECTION('center_axis',(-1.,0.,0.));
#4579=DIRECTION('ref_axis',(0.,0.,1.));
#4580=DIRECTION('center_axis',(1.,0.,0.));
#4581=DIRECTION('ref_axis',(0.,0.,-1.));
#4582=DIRECTION('center_axis',(1.,0.,0.));
#4583=DIRECTION('ref_axis',(0.,0.,-1.));
#4584=DIRECTION('center_axis',(0.,-1.,-1.22464679914735E-16));
#4585=DIRECTION('ref_axis',(0.,-1.22464679914735E-16,1.));
#4586=DIRECTION('center_axis',(1.,0.,0.));
#4587=DIRECTION('ref_axis',(0.,1.22464679914735E-16,1.));
#4588=DIRECTION('center_axis',(-1.,0.,0.));
#4589=DIRECTION('ref_axis',(0.,0.,1.));
#4590=DIRECTION('axis',(0.,0.,1.));
#4591=DIRECTION('refdir',(1.,0.,0.));
#4592=DIRECTION('center_axis',(1.,0.,0.));
#4593=DIRECTION('ref_axis',(0.,0.,-1.));
#4594=DIRECTION('center_axis',(-1.,0.,0.));
#4595=DIRECTION('ref_axis',(0.,1.22464679914735E-16,1.));
#4596=DIRECTION('center_axis',(0.,-1.,-1.22464679914735E-16));
#4597=DIRECTION('ref_axis',(0.,-1.22464679914735E-16,1.));
#4598=DIRECTION('center_axis',(1.,0.,0.));
#4599=DIRECTION('ref_axis',(0.,0.,1.));
#4600=DIRECTION('center_axis',(1.,0.,0.));
#4601=DIRECTION('ref_axis',(0.,0.,-1.));
#4602=DIRECTION('',(-0.999999956307574,3.62016965808782E-20,-0.000295609285927038));
#4603=DIRECTION('center_axis',(-1.,0.,0.));
#4604=DIRECTION('ref_axis',(0.,0.,1.));
#4605=DIRECTION('center_axis',(1.,0.,0.));
#4606=DIRECTION('ref_axis',(0.,0.,-1.));
#4607=DIRECTION('center_axis',(1.,0.,0.));
#4608=DIRECTION('ref_axis',(0.,0.,-1.));
#4609=DIRECTION('center_axis',(0.,-1.,-1.22464679914735E-16));
#4610=DIRECTION('ref_axis',(0.,-1.22464679914735E-16,1.));
#4611=DIRECTION('center_axis',(1.,0.,0.));
#4612=DIRECTION('ref_axis',(0.,1.22464679914735E-16,1.));
#4613=DIRECTION('center_axis',(-1.,0.,0.));
#4614=DIRECTION('ref_axis',(0.,0.,1.));
#4615=DIRECTION('axis',(0.,0.,1.));
#4616=DIRECTION('refdir',(1.,0.,0.));
#4617=DIRECTION('center_axis',(0.,1.,0.));
#4618=DIRECTION('ref_axis',(0.,0.,1.));
#4619=DIRECTION('',(0.,0.,1.));
#4620=DIRECTION('',(1.,0.,0.));
#4621=DIRECTION('',(1.,0.,0.));
#4622=DIRECTION('',(1.,0.,0.));
#4623=DIRECTION('',(1.,0.,0.));
#4624=DIRECTION('',(1.,0.,0.));
#4625=DIRECTION('',(1.,0.,0.));
#4626=DIRECTION('',(1.,0.,0.));
#4627=DIRECTION('',(1.,0.,0.));
#4628=DIRECTION('',(1.,0.,0.));
#4629=DIRECTION('',(1.,0.,0.));
#4630=DIRECTION('',(1.,0.,0.));
#4631=DIRECTION('',(1.,0.,0.));
#4632=DIRECTION('',(1.,0.,0.));
#4633=DIRECTION('',(0.,0.,1.));
#4634=DIRECTION('',(-1.,0.,0.));
#4635=DIRECTION('',(-1.,0.,0.));
#4636=DIRECTION('',(-1.,0.,0.));
#4637=DIRECTION('',(-1.,0.,0.));
#4638=DIRECTION('',(-1.,0.,0.));
#4639=DIRECTION('',(-1.,0.,0.));
#4640=DIRECTION('',(-1.,0.,0.));
#4641=DIRECTION('',(-1.,0.,0.));
#4642=DIRECTION('',(-1.,0.,0.));
#4643=DIRECTION('',(-1.,0.,0.));
#4644=DIRECTION('',(-1.,0.,0.));
#4645=DIRECTION('',(-1.,0.,0.));
#4646=DIRECTION('',(-1.,0.,0.));
#4647=DIRECTION('center_axis',(0.,-1.,0.));
#4648=DIRECTION('ref_axis',(0.,0.,-1.));
#4649=DIRECTION('',(1.,0.,0.));
#4650=DIRECTION('',(1.,0.,0.));
#4651=DIRECTION('',(1.,0.,0.));
#4652=DIRECTION('',(1.,0.,0.));
#4653=DIRECTION('',(1.,0.,0.));
#4654=DIRECTION('',(1.,0.,0.));
#4655=DIRECTION('',(1.,0.,0.));
#4656=DIRECTION('',(1.,0.,0.));
#4657=DIRECTION('',(1.,0.,0.));
#4658=DIRECTION('',(1.,0.,0.));
#4659=DIRECTION('',(1.,0.,0.));
#4660=DIRECTION('',(1.,0.,0.));
#4661=DIRECTION('',(1.,0.,0.));
#4662=DIRECTION('',(0.,0.,-1.));
#4663=DIRECTION('',(-1.,0.,0.));
#4664=DIRECTION('',(-1.,0.,0.));
#4665=DIRECTION('',(-1.,0.,0.));
#4666=DIRECTION('',(-1.,0.,0.));
#4667=DIRECTION('',(-1.,0.,0.));
#4668=DIRECTION('',(-1.,0.,0.));
#4669=DIRECTION('',(-1.,0.,0.));
#4670=DIRECTION('',(-1.,0.,0.));
#4671=DIRECTION('',(-1.,0.,0.));
#4672=DIRECTION('',(-1.,0.,0.));
#4673=DIRECTION('',(-1.,0.,0.));
#4674=DIRECTION('',(-1.,0.,0.));
#4675=DIRECTION('',(-1.,0.,0.));
#4676=DIRECTION('',(0.,0.,-1.));
#4677=DIRECTION('center_axis',(-1.,0.,0.));
#4678=DIRECTION('ref_axis',(0.,-1.,2.19773242311135E-14));
#4679=DIRECTION('center_axis',(-1.,0.,0.));
#4680=DIRECTION('ref_axis',(0.,-1.,2.19773242311135E-14));
#4681=DIRECTION('center_axis',(-1.,0.,0.));
#4682=DIRECTION('ref_axis',(0.,-1.,2.19773242311135E-14));
#4683=DIRECTION('center_axis',(-1.,0.,0.));
#4684=DIRECTION('ref_axis',(0.,-1.,2.19773242311135E-14));
#4685=DIRECTION('center_axis',(-1.,0.,0.));
#4686=DIRECTION('ref_axis',(0.,-1.,2.19773242311135E-14));
#4687=DIRECTION('center_axis',(-1.,0.,0.));
#4688=DIRECTION('ref_axis',(0.,-1.,2.19773242311135E-14));
#4689=DIRECTION('center_axis',(-1.,0.,0.));
#4690=DIRECTION('ref_axis',(0.,-1.,2.19773242311135E-14));
#4691=DIRECTION('center_axis',(-1.,0.,0.));
#4692=DIRECTION('ref_axis',(0.,-1.,2.19773242311135E-14));
#4693=DIRECTION('center_axis',(-1.,0.,0.));
#4694=DIRECTION('ref_axis',(0.,-1.,2.19773242311135E-14));
#4695=DIRECTION('center_axis',(-1.,0.,0.));
#4696=DIRECTION('ref_axis',(0.,-1.,2.19773242311135E-14));
#4697=DIRECTION('center_axis',(-1.,0.,0.));
#4698=DIRECTION('ref_axis',(0.,-1.,2.19773242311135E-14));
#4699=DIRECTION('center_axis',(-1.,0.,0.));
#4700=DIRECTION('ref_axis',(0.,-1.,2.19773242311135E-14));
#4701=DIRECTION('center_axis',(-1.,0.,0.));
#4702=DIRECTION('ref_axis',(0.,-1.,2.19773242311135E-14));
#4703=DIRECTION('center_axis',(-1.,0.,0.));
#4704=DIRECTION('ref_axis',(0.,-1.,2.19773242311135E-14));
#4705=DIRECTION('center_axis',(-1.,0.,0.));
#4706=DIRECTION('ref_axis',(0.,-1.,2.19773242311135E-14));
#4707=DIRECTION('center_axis',(1.,0.,0.));
#4708=DIRECTION('ref_axis',(0.,-1.,2.19773242311135E-14));
#4709=DIRECTION('center_axis',(1.,2.26944640896891E-13,2.4756931710509E-13));
#4710=DIRECTION('ref_axis',(-2.99635666187295E-14,0.794492776111595,-0.607273602840179));
#4711=DIRECTION('center_axis',(1.,-4.24721344664965E-14,7.81460509822211E-14));
#4712=DIRECTION('ref_axis',(-1.5231504897179E-14,0.783860772073074,0.620936623179052));
#4713=DIRECTION('center_axis',(-1.,0.,0.));
#4714=DIRECTION('ref_axis',(0.,-1.,0.));
#4715=DIRECTION('center_axis',(1.,0.,0.));
#4716=DIRECTION('ref_axis',(0.,-1.,0.));
#4717=DIRECTION('center_axis',(-1.,0.,0.));
#4718=DIRECTION('ref_axis',(0.,-1.,0.));
#4719=DIRECTION('center_axis',(-1.,0.,0.));
#4720=DIRECTION('ref_axis',(0.,-1.,0.));
#4721=DIRECTION('center_axis',(1.,0.,0.));
#4722=DIRECTION('ref_axis',(0.,-1.,0.));
#4723=DIRECTION('center_axis',(-1.,0.,0.));
#4724=DIRECTION('ref_axis',(0.,-1.,0.));
#4725=DIRECTION('center_axis',(-1.,0.,0.));
#4726=DIRECTION('ref_axis',(0.,-1.,0.));
#4727=DIRECTION('center_axis',(-1.,0.,0.));
#4728=DIRECTION('ref_axis',(0.,-1.,0.));
#4729=DIRECTION('center_axis',(-1.,0.,0.));
#4730=DIRECTION('ref_axis',(0.,-1.,0.));
#4731=DIRECTION('center_axis',(-1.,0.,0.));
#4732=DIRECTION('ref_axis',(0.,-1.,0.));
#4733=DIRECTION('center_axis',(-1.,0.,0.));
#4734=DIRECTION('ref_axis',(0.,-1.,0.));
#4735=DIRECTION('center_axis',(-1.,0.,0.));
#4736=DIRECTION('ref_axis',(0.,-1.,0.));
#4737=DIRECTION('center_axis',(-1.,0.,0.));
#4738=DIRECTION('ref_axis',(0.,-1.,0.));
#4739=DIRECTION('center_axis',(-1.,0.,0.));
#4740=DIRECTION('ref_axis',(0.,-1.,0.));
#4741=DIRECTION('center_axis',(-1.,0.,0.));
#4742=DIRECTION('ref_axis',(0.,-1.,0.));
#4743=DIRECTION('center_axis',(-1.,0.,0.));
#4744=DIRECTION('ref_axis',(0.,-1.,0.));
#4745=DIRECTION('center_axis',(-1.,0.,0.));
#4746=DIRECTION('ref_axis',(0.,-1.,0.));
#4747=DIRECTION('center_axis',(1.,-7.18663344203148E-15,1.44094323913819E-14));
#4748=DIRECTION('ref_axis',(-4.36221174028664E-15,0.74050159851997,0.672054597922944));
#4749=DIRECTION('center_axis',(1.,-2.70011984489144E-13,-2.93694733491497E-13));
#4750=DIRECTION('ref_axis',(4.40921431182727E-14,-0.656854870457007,0.754017028426354));
#4751=DIRECTION('center_axis',(1.,0.,0.));
#4752=DIRECTION('ref_axis',(0.,-1.,0.));
#4753=DIRECTION('center_axis',(1.,0.,0.));
#4754=DIRECTION('ref_axis',(0.,-1.,0.));
#4755=DIRECTION('',(-1.,0.,0.));
#4756=DIRECTION('center_axis',(-1.,0.,0.));
#4757=DIRECTION('ref_axis',(0.,-1.,0.));
#4758=DIRECTION('center_axis',(-1.,0.,0.));
#4759=DIRECTION('ref_axis',(0.,-1.,0.));
#4760=DIRECTION('center_axis',(-1.,0.,0.));
#4761=DIRECTION('ref_axis',(0.,-1.,0.));
#4762=DIRECTION('axis',(0.,0.,1.));
#4763=DIRECTION('refdir',(1.,0.,0.));
#4764=DIRECTION('center_axis',(1.,0.,0.));
#4765=DIRECTION('ref_axis',(0.,0.,-1.));
#4766=DIRECTION('center_axis',(1.,0.,0.));
#4767=DIRECTION('ref_axis',(0.,0.,-1.));
#4768=DIRECTION('',(1.,0.,0.));
#4769=DIRECTION('center_axis',(1.,0.,0.));
#4770=DIRECTION('ref_axis',(0.,0.,-1.));
#4771=DIRECTION('center_axis',(1.,0.,0.));
#4772=DIRECTION('ref_axis',(0.,0.,-1.));
#4773=DIRECTION('center_axis',(1.,0.,0.));
#4774=DIRECTION('ref_axis',(0.,0.,-1.));
#4775=DIRECTION('center_axis',(1.,0.,0.));
#4776=DIRECTION('ref_axis',(0.,0.,-1.));
#4777=DIRECTION('center_axis',(0.,-1.,-1.22464679914735E-16));
#4778=DIRECTION('ref_axis',(0.,-1.22464679914735E-16,1.));
#4779=DIRECTION('center_axis',(1.,0.,0.));
#4780=DIRECTION('ref_axis',(0.,0.,-1.));
#4781=DIRECTION('center_axis',(-1.,0.,0.));
#4782=DIRECTION('ref_axis',(0.,0.,-1.));
#4783=DIRECTION('center_axis',(0.,-1.,-1.22464679914735E-16));
#4784=DIRECTION('ref_axis',(0.,-1.22464679914735E-16,1.));
#4785=DIRECTION('center_axis',(1.,0.,0.));
#4786=DIRECTION('ref_axis',(0.,0.,-1.));
#4787=DIRECTION('center_axis',(-1.,0.,0.));
#4788=DIRECTION('ref_axis',(0.,0.,1.));
#4789=DIRECTION('center_axis',(1.,0.,0.));
#4790=DIRECTION('ref_axis',(0.,0.,-1.));
#4791=DIRECTION('center_axis',(1.,0.,0.));
#4792=DIRECTION('ref_axis',(0.,0.,-1.));
#4793=DIRECTION('',(1.,0.,0.));
#4794=DIRECTION('center_axis',(1.,0.,0.));
#4795=DIRECTION('ref_axis',(0.,0.,-1.));
#4796=DIRECTION('center_axis',(1.,0.,0.));
#4797=DIRECTION('ref_axis',(0.,0.,-1.));
#4798=DIRECTION('',(1.,0.,0.));
#4799=DIRECTION('center_axis',(-1.,0.,0.));
#4800=DIRECTION('ref_axis',(0.,0.,-1.));
#4801=DIRECTION('center_axis',(1.,0.,0.));
#4802=DIRECTION('ref_axis',(0.,0.,-1.));
#4803=DIRECTION('center_axis',(1.,0.,0.));
#4804=DIRECTION('ref_axis',(0.,0.,-1.));
#4805=DIRECTION('',(-0.776187356563468,7.72142659683039E-17,-0.630502329504829));
#4806=DIRECTION('center_axis',(1.,0.,0.));
#4807=DIRECTION('ref_axis',(0.,0.,-1.));
#4808=DIRECTION('center_axis',(-1.,0.,0.));
#4809=DIRECTION('ref_axis',(0.,0.,1.));
#4810=DIRECTION('center_axis',(1.,0.,0.));
#4811=DIRECTION('ref_axis',(0.,0.,-1.));
#4812=DIRECTION('center_axis',(1.,0.,0.));
#4813=DIRECTION('ref_axis',(0.,0.,-1.));
#4814=DIRECTION('',(-1.,0.,0.));
#4815=DIRECTION('center_axis',(-1.,0.,0.));
#4816=DIRECTION('ref_axis',(0.,0.,-1.));
#4817=DIRECTION('',(0.689249232259327,-8.87286394090086E-17,-0.724524323835942));
#4818=DIRECTION('center_axis',(1.,0.,0.));
#4819=DIRECTION('ref_axis',(0.,0.,-1.));
#4820=DIRECTION('center_axis',(1.,0.,0.));
#4821=DIRECTION('ref_axis',(0.,0.,-1.));
#4822=DIRECTION('axis',(0.,0.,1.));
#4823=DIRECTION('refdir',(1.,0.,0.));
#4824=DIRECTION('',(1.,0.,0.));
#4825=DIRECTION('',(1.,0.,0.));
#4826=DIRECTION('center_axis',(1.,0.,0.));
#4827=DIRECTION('ref_axis',(0.,0.444750988585694,0.895654262621492));
#4828=DIRECTION('center_axis',(-1.,0.,0.));
#4829=DIRECTION('ref_axis',(0.,0.444750988585694,0.895654262621492));
#4830=DIRECTION('center_axis',(-1.,0.,0.));
#4831=DIRECTION('ref_axis',(0.,0.444750988585694,0.895654262621492));
#4832=DIRECTION('',(1.,0.,0.));
#4833=DIRECTION('',(1.,0.,0.));
#4834=DIRECTION('center_axis',(1.,0.,0.));
#4835=DIRECTION('ref_axis',(0.,-0.580623944517215,-0.814171870708679));
#4836=DIRECTION('center_axis',(-1.,0.,0.));
#4837=DIRECTION('ref_axis',(0.,-0.580623944517215,-0.814171870708679));
#4838=DIRECTION('center_axis',(-1.,0.,0.));
#4839=DIRECTION('ref_axis',(0.,-0.580623944517215,-0.814171870708679));
#4840=DIRECTION('center_axis',(0.,0.866025403784439,0.5));
#4841=DIRECTION('ref_axis',(0.,-0.5,0.866025403784439));
#4842=DIRECTION('',(0.,-0.5,0.866025403784439));
#4843=DIRECTION('',(1.,0.,0.));
#4844=DIRECTION('',(0.,-0.5,0.866025403784439));
#4845=DIRECTION('',(1.,0.,0.));
#4846=DIRECTION('center_axis',(0.,0.866025403784438,-0.5));
#4847=DIRECTION('ref_axis',(0.,0.5,0.866025403784438));
#4848=DIRECTION('',(0.,0.5,0.866025403784438));
#4849=DIRECTION('',(0.,0.5,0.866025403784438));
#4850=DIRECTION('',(1.,0.,0.));
#4851=DIRECTION('center_axis',(0.,-3.02823770847138E-16,-1.));
#4852=DIRECTION('ref_axis',(0.,1.,-3.02823770847138E-16));
#4853=DIRECTION('',(0.,1.,-3.02823770847138E-16));
#4854=DIRECTION('',(0.,1.,-3.02823770847138E-16));
#4855=DIRECTION('',(1.,0.,0.));
#4856=DIRECTION('center_axis',(0.,-0.866025403784439,-0.5));
#4857=DIRECTION('ref_axis',(0.,0.5,-0.866025403784439));
#4858=DIRECTION('',(0.,0.5,-0.866025403784439));
#4859=DIRECTION('',(0.,0.5,-0.866025403784439));
#4860=DIRECTION('',(1.,0.,0.));
#4861=DIRECTION('center_axis',(0.,-0.866025403784439,0.5));
#4862=DIRECTION('ref_axis',(0.,-0.5,-0.866025403784439));
#4863=DIRECTION('',(0.,-0.5,-0.866025403784439));
#4864=DIRECTION('',(0.,-0.5,-0.866025403784439));
#4865=DIRECTION('',(1.,0.,0.));
#4866=DIRECTION('center_axis',(0.,6.05647541694275E-16,1.));
#4867=DIRECTION('ref_axis',(0.,-1.,6.05647541694275E-16));
#4868=DIRECTION('',(0.,-1.,6.05647541694275E-16));
#4869=DIRECTION('',(0.,-1.,6.05647541694275E-16));
#4870=DIRECTION('center_axis',(1.,0.,0.));
#4871=DIRECTION('ref_axis',(0.,1.,0.));
#4872=DIRECTION('center_axis',(1.,0.,0.));
#4873=DIRECTION('ref_axis',(0.,1.,0.));
#4874=DIRECTION('axis',(0.,0.,1.));
#4875=DIRECTION('refdir',(1.,0.,0.));
#4876=DIRECTION('center_axis',(0.,1.46957615897682E-15,1.));
#4877=DIRECTION('ref_axis',(1.,0.,0.));
#4878=DIRECTION('center_axis',(0.,0.,1.));
#4879=DIRECTION('ref_axis',(1.,0.,0.));
#4880=DIRECTION('',(0.,0.,1.));
#4881=DIRECTION('',(1.,0.,0.));
#4882=DIRECTION('',(0.,0.,1.));
#4883=DIRECTION('',(1.,0.,0.));
#4884=DIRECTION('',(0.,0.,1.));
#4885=DIRECTION('',(1.,0.,0.));
#4886=DIRECTION('',(0.,0.,1.));
#4887=DIRECTION('',(1.,0.,0.));
#4888=DIRECTION('',(0.,0.,1.));
#4889=DIRECTION('',(1.,0.,0.));
#4890=DIRECTION('',(0.,0.,1.));
#4891=DIRECTION('',(1.,0.,0.));
#4892=DIRECTION('',(0.,0.,1.));
#4893=DIRECTION('',(1.,0.,0.));
#4894=DIRECTION('',(0.,0.,1.));
#4895=DIRECTION('',(1.,0.,0.));
#4896=DIRECTION('',(0.,0.,1.));
#4897=DIRECTION('',(1.,0.,0.));
#4898=DIRECTION('',(0.,0.,1.));
#4899=DIRECTION('',(1.,0.,0.));
#4900=CARTESIAN_POINT('',(0.,0.,0.));
#4901=CARTESIAN_POINT('',(0.,0.,0.));
#4902=CARTESIAN_POINT('Origin',(15.8714473032184,0.,0.));
#4903=CARTESIAN_POINT('',(15.8714473032184,3.29760625124175,0.999999999999998));
#4904=CARTESIAN_POINT('',(14.8714473032184,3.44589712386029,-6.01983033610089E-17));
#4905=CARTESIAN_POINT('Ctrl Pts',(15.8714473032184,3.29760625124174,0.999999999999999));
#4906=CARTESIAN_POINT('Ctrl Pts',(15.9978139569531,3.29760625124174,0.999999999999999));
#4907=CARTESIAN_POINT('Ctrl Pts',(16.132068844028,3.30562953237115,0.974596096350375));
#4908=CARTESIAN_POINT('Ctrl Pts',(16.3782103010389,3.33407731229027,0.872325929581351));
#4909=CARTESIAN_POINT('Ctrl Pts',(16.4901654582252,3.3540348875684,0.795495407366277));
#4910=CARTESIAN_POINT('Ctrl Pts',(16.6669197871454,3.39109395594973,0.618741078446085));
#4911=CARTESIAN_POINT('Ctrl Pts',(16.7437680872924,3.41067812574963,0.506776556958312));
#4912=CARTESIAN_POINT('Ctrl Pts',(16.8460513462857,3.43826042485992,0.26060123975522));
#4913=CARTESIAN_POINT('Ctrl Pts',(16.8714473032184,3.44589712386029,0.126333880758864));
#4914=CARTESIAN_POINT('Ctrl Pts',(16.8714473032184,3.44589712386029,-0.126333880758864));
#4915=CARTESIAN_POINT('Ctrl Pts',(16.8460513462857,3.43826042485992,-0.260601239755222));
#4916=CARTESIAN_POINT('Ctrl Pts',(16.7437680872924,3.41067812574963,-0.506776556958312));
#4917=CARTESIAN_POINT('Ctrl Pts',(16.6669197871454,3.39109395594973,-0.618741078446085));
#4918=CARTESIAN_POINT('Ctrl Pts',(16.4901654582252,3.3540348875684,-0.795495407366277));
#4919=CARTESIAN_POINT('Ctrl Pts',(16.3782103010389,3.33407731229027,-0.872325929581349));
#4920=CARTESIAN_POINT('Ctrl Pts',(16.132068844028,3.30562953237115,-0.974596096350375));
#4921=CARTESIAN_POINT('Ctrl Pts',(15.9978139569531,3.29760625124174,-0.999999999999999));
#4922=CARTESIAN_POINT('Ctrl Pts',(15.7450806494837,3.29760625124174,-0.999999999999999));
#4923=CARTESIAN_POINT('Ctrl Pts',(15.6108257624088,3.30562953237115,-0.974596096350376));
#4924=CARTESIAN_POINT('Ctrl Pts',(15.3646843053979,3.33407731229027,-0.872325929581351));
#4925=CARTESIAN_POINT('Ctrl Pts',(15.2527291482116,3.3540348875684,-0.795495407366277));
#4926=CARTESIAN_POINT('Ctrl Pts',(15.0759748192914,3.39109395594973,-0.618741078446085));
#4927=CARTESIAN_POINT('Ctrl Pts',(14.9991265191444,3.41067812574963,-0.506776556958314));
#4928=CARTESIAN_POINT('Ctrl Pts',(14.8968432601511,3.43826042485992,-0.260601239755224));
#4929=CARTESIAN_POINT('Ctrl Pts',(14.8714473032184,3.44589712386029,-0.126333880758864));
#4930=CARTESIAN_POINT('Ctrl Pts',(14.8714473032184,3.44589712386029,-2.42861286636753E-16));
#4931=CARTESIAN_POINT('Ctrl Pts',(14.8714473032184,3.44589712386029,-1.38777878078145E-16));
#4932=CARTESIAN_POINT('Ctrl Pts',(14.8714473032184,3.44589712386029,0.126333880758864));
#4933=CARTESIAN_POINT('Ctrl Pts',(14.8968432601511,3.43826042485992,0.260601239755221));
#4934=CARTESIAN_POINT('Ctrl Pts',(14.9991265191444,3.41067812574963,0.506776556958312));
#4935=CARTESIAN_POINT('Ctrl Pts',(15.0759748192914,3.39109395594973,0.618741078446085));
#4936=CARTESIAN_POINT('Ctrl Pts',(15.2527291482116,3.3540348875684,0.795495407366277));
#4937=CARTESIAN_POINT('Ctrl Pts',(15.3646843053979,3.33407731229027,0.872325929581349));
#4938=CARTESIAN_POINT('Ctrl Pts',(15.6108257624088,3.30562953237115,0.974596096350375));
#4939=CARTESIAN_POINT('Ctrl Pts',(15.7450806494837,3.29760625124174,0.999999999999999));
#4940=CARTESIAN_POINT('Ctrl Pts',(15.8714473032184,3.29760625124174,0.999999999999999));
#4941=CARTESIAN_POINT('',(14.8714473032184,7.52312685038423,1.22464679914735E-16));
#4942=CARTESIAN_POINT('',(14.8714473032184,0.,1.22464679914735E-16));
#4943=CARTESIAN_POINT('',(15.8714473032184,7.45636892910833,0.999999999999999));
#4944=CARTESIAN_POINT('Ctrl Pts',(15.8714473032184,7.45636892910833,0.999999999999999));
#4945=CARTESIAN_POINT('Ctrl Pts',(15.7457245010652,7.45636892910833,0.999999999999999));
#4946=CARTESIAN_POINT('Ctrl Pts',(15.6117245964979,7.45987689127736,0.974843764196788));
#4947=CARTESIAN_POINT('Ctrl Pts',(15.3653900481838,7.47250970222183,0.872744136330349));
#4948=CARTESIAN_POINT('Ctrl Pts',(15.2530425360435,7.48144799782428,0.795808795198177));
#4949=CARTESIAN_POINT('Ctrl Pts',(15.0756394573932,7.49819644864561,0.618405716547907));
#4950=CARTESIAN_POINT('Ctrl Pts',(14.9987033720303,7.50710016352641,0.506057792670463));
#4951=CARTESIAN_POINT('Ctrl Pts',(14.8966032000273,7.51965370990447,0.259721846141313));
#4952=CARTESIAN_POINT('Ctrl Pts',(14.8714473032184,7.52312685038423,0.125721456548635));
#4953=CARTESIAN_POINT('Ctrl Pts',(14.8714473032184,7.52312685038423,-1.04083408558608E-16));
#4954=CARTESIAN_POINT('Ctrl Pts',(14.8714473032184,7.52312685038423,-2.08166817117217E-16));
#4955=CARTESIAN_POINT('Ctrl Pts',(14.8714473032184,7.52312685038423,-0.125721456548636));
#4956=CARTESIAN_POINT('Ctrl Pts',(14.8966032000273,7.51965370990447,-0.259721846141313));
#4957=CARTESIAN_POINT('Ctrl Pts',(14.9987033720303,7.50710016352641,-0.506057792670463));
#4958=CARTESIAN_POINT('Ctrl Pts',(15.0756394573932,7.49819644864561,-0.618405716547907));
#4959=CARTESIAN_POINT('Ctrl Pts',(15.2530425360435,7.48144799782428,-0.795808795198177));
#4960=CARTESIAN_POINT('Ctrl Pts',(15.3653900481838,7.47250970222183,-0.872744136330348));
#4961=CARTESIAN_POINT('Ctrl Pts',(15.6117245964979,7.45987689127736,-0.974843764196788));
#4962=CARTESIAN_POINT('Ctrl Pts',(15.7457245010652,7.45636892910833,-0.999999999999999));
#4963=CARTESIAN_POINT('Ctrl Pts',(15.9971701053716,7.45636892910833,-0.999999999999999));
#4964=CARTESIAN_POINT('Ctrl Pts',(16.1311700099389,7.45987689127736,-0.974843764196788));
#4965=CARTESIAN_POINT('Ctrl Pts',(16.377504558253,7.47250970222183,-0.872744136330349));
#4966=CARTESIAN_POINT('Ctrl Pts',(16.4898520703933,7.48144799782428,-0.795808795198177));
#4967=CARTESIAN_POINT('Ctrl Pts',(16.6672551490436,7.49819644864561,-0.618405716547907));
#4968=CARTESIAN_POINT('Ctrl Pts',(16.7441912344065,7.50710016352641,-0.506057792670463));
#4969=CARTESIAN_POINT('Ctrl Pts',(16.8462914064095,7.51965370990447,-0.259721846141313));
#4970=CARTESIAN_POINT('Ctrl Pts',(16.8714473032184,7.52312685038423,-0.125721456548635));
#4971=CARTESIAN_POINT('Ctrl Pts',(16.8714473032184,7.52312685038423,0.125721456548635));
#4972=CARTESIAN_POINT('Ctrl Pts',(16.8462914064095,7.51965370990447,0.259721846141313));
#4973=CARTESIAN_POINT('Ctrl Pts',(16.7441912344065,7.50710016352641,0.506057792670463));
#4974=CARTESIAN_POINT('Ctrl Pts',(16.6672551490436,7.49819644864561,0.618405716547907));
#4975=CARTESIAN_POINT('Ctrl Pts',(16.4898520703933,7.48144799782428,0.795808795198176));
#4976=CARTESIAN_POINT('Ctrl Pts',(16.377504558253,7.47250970222183,0.872744136330349));
#4977=CARTESIAN_POINT('Ctrl Pts',(16.1311700099389,7.45987689127736,0.974843764196788));
#4978=CARTESIAN_POINT('Ctrl Pts',(15.9971701053716,7.45636892910833,0.999999999999999));
#4979=CARTESIAN_POINT('Ctrl Pts',(15.8714473032184,7.45636892910833,0.999999999999999));
#4980=CARTESIAN_POINT('Origin',(11.0238490761438,0.,0.));
#4981=CARTESIAN_POINT('',(11.0238490761438,5.,-6.12323399573677E-16));
#4982=CARTESIAN_POINT('Origin',(11.0238490761438,0.,0.));
#4983=CARTESIAN_POINT('',(12.0767011645438,5.,-6.12323399573677E-16));
#4984=CARTESIAN_POINT('',(11.0238490761438,5.,6.12323399573677E-16));
#4985=CARTESIAN_POINT('Origin',(12.0767011645438,0.,0.));
#4986=CARTESIAN_POINT('Origin',(12.0767011645438,0.,0.));
#4987=CARTESIAN_POINT('',(12.076701164516,-4.22000688292658E-16,3.44589712386029));
#4988=CARTESIAN_POINT('Origin',(12.076701164516,0.,0.));
#4989=CARTESIAN_POINT('Origin',(11.474739121518,0.,0.));
#4990=CARTESIAN_POINT('',(11.9256291668923,-9.21317321690256E-16,7.52312685038423));
#4991=CARTESIAN_POINT('Origin',(11.9256291668923,0.,0.));
#4992=CARTESIAN_POINT('',(11.0238490761438,-8.44001376585316E-16,6.89179424772059));
#4993=CARTESIAN_POINT('',(11.474739121518,-8.82659349137786E-16,7.20746054905241));
#4994=CARTESIAN_POINT('Origin',(11.0238490761438,0.,0.));
#4995=CARTESIAN_POINT('Origin',(16.3019119808107,0.,0.));
#4996=CARTESIAN_POINT('',(20.6781947947292,-9.21317321690256E-16,7.52312685038423));
#4997=CARTESIAN_POINT('Origin',(20.6781947947292,0.,0.));
#4998=CARTESIAN_POINT('',(16.3019119808107,-9.21317321690256E-16,7.52312685038423));
#4999=CARTESIAN_POINT('Origin',(20.9315098273138,0.,0.));
#5000=CARTESIAN_POINT('',(21.1848248598985,-8.82659349137786E-16,7.20746054905241));
#5001=CARTESIAN_POINT('',(20.9315098273138,9.01988335414021E-16,7.36529369971832));
#5002=CARTESIAN_POINT('Origin',(21.1848248598985,0.,0.));
#5003=CARTESIAN_POINT('Origin',(21.4140009475395,0.,0.));
#5004=CARTESIAN_POINT('',(21.6431770351805,-9.21957102532866E-16,7.52835105742136));
#5005=CARTESIAN_POINT('Origin',(21.6431770351805,0.,0.));
#5006=CARTESIAN_POINT('',(21.4140009475395,-9.02308225835327E-16,7.36790580323689));
#5007=CARTESIAN_POINT('Origin',(48.2427605064424,0.,0.));
#5008=CARTESIAN_POINT('',(74.8423439777042,-9.21957102532866E-16,7.52835105742136));
#5009=CARTESIAN_POINT('Origin',(74.8423439777042,0.,0.));
#5010=CARTESIAN_POINT('',(48.2427605064424,-9.21957102532866E-16,7.52835105742136));
#5011=CARTESIAN_POINT('Origin',(75.5565470559241,0.,0.));
#5012=CARTESIAN_POINT('',(76.270750134144,-7.86576021887409E-16,6.42288064146376));
#5013=CARTESIAN_POINT('',(75.5565470559241,8.54266562210138E-16,6.97561584944256));
#5014=CARTESIAN_POINT('Origin',(76.270750134144,0.,0.));
#5015=CARTESIAN_POINT('Origin',(53.9616500647475,0.,0.));
#5016=CARTESIAN_POINT('',(31.6525499953511,-7.84960767273423E-16,6.40969108660508));
#5017=CARTESIAN_POINT('Origin',(31.6525499953511,0.,0.));
#5018=CARTESIAN_POINT('',(53.9616500647475,-7.85768394580416E-16,6.41628586403442));
#5019=CARTESIAN_POINT('Origin',(31.0318089645314,0.,0.));
#5020=CARTESIAN_POINT('',(30.4110679337117,-7.84960767273423E-16,6.40969108660508));
#5021=CARTESIAN_POINT('Origin',(30.4110679337117,0.,0.));
#5022=CARTESIAN_POINT('',(31.0318089645314,-7.84960767273423E-16,6.40969108660508));
#5023=CARTESIAN_POINT('Origin',(29.5420239984498,0.,0.));
#5024=CARTESIAN_POINT('',(28.6729800631879,-7.84852901782084E-16,6.40881029802658));
#5025=CARTESIAN_POINT('Origin',(28.6729800631879,0.,0.));
#5026=CARTESIAN_POINT('',(29.5420239984498,-7.84884362648318E-16,6.40906719549494));
#5027=CARTESIAN_POINT('Origin',(28.6729800631879,0.,-6.41550316824698));
#5028=CARTESIAN_POINT('',(28.6729800631879,-7.85672541991337E-16,6.41550316824698));
#5029=CARTESIAN_POINT('Origin',(28.6729800631879,0.,0.));
#5030=CARTESIAN_POINT('Origin',(28.2136282688352,0.,0.));
#5031=CARTESIAN_POINT('',(27.7542764744824,-7.85672541991337E-16,6.41550316824698));
#5032=CARTESIAN_POINT('Origin',(27.7542764744824,0.,0.));
#5033=CARTESIAN_POINT('',(28.2136282688352,-7.85672541991337E-16,6.41550316824698));
#5034=CARTESIAN_POINT('Origin',(27.7542764744824,0.,-6.40853872070288));
#5035=CARTESIAN_POINT('',(27.7542764744824,-7.84819643152065E-16,6.40853872070288));
#5036=CARTESIAN_POINT('Origin',(27.7542764744824,0.,0.));
#5037=CARTESIAN_POINT('Origin',(26.6245076505395,0.,0.));
#5038=CARTESIAN_POINT('',(25.4947388265965,-7.84737844052149E-16,6.40787078036307));
#5039=CARTESIAN_POINT('Origin',(25.4947388265965,0.,0.));
#5040=CARTESIAN_POINT('',(26.6245076505395,-7.84778743602106E-16,6.40820475053297));
#5041=CARTESIAN_POINT('Origin',(25.0105689136245,0.,0.));
#5042=CARTESIAN_POINT('',(24.5263990006525,-7.84737844052149E-16,6.40787078036307));
#5043=CARTESIAN_POINT('Origin',(24.5263990006525,0.,0.));
#5044=CARTESIAN_POINT('',(25.0105689136245,-7.84737844052149E-16,6.40787078036307));
#5045=CARTESIAN_POINT('Origin',(23.6497386319918,0.,0.));
#5046=CARTESIAN_POINT('',(22.7730782633312,-7.84639315317936E-16,6.40706623219228));
#5047=CARTESIAN_POINT('Origin',(22.7730782633312,0.,0.));
#5048=CARTESIAN_POINT('',(23.6497386319918,-7.84671051911994E-16,6.40732538114918));
#5049=CARTESIAN_POINT('Origin',(22.2310089528171,0.,0.));
#5050=CARTESIAN_POINT('',(21.688939642303,-7.84639315317937E-16,6.40706623219228));
#5051=CARTESIAN_POINT('Origin',(21.688939642303,0.,0.));
#5052=CARTESIAN_POINT('',(22.2310089528171,-7.84639315317937E-16,6.40706623219228));
#5053=CARTESIAN_POINT('Origin',(21.4368822511007,0.,0.));
#5054=CARTESIAN_POINT('',(21.1848248598985,-7.8458181784762E-16,6.4065967297173));
#5055=CARTESIAN_POINT('Origin',(21.1848248598985,0.,0.));
#5056=CARTESIAN_POINT('',(21.4368822511007,-7.84590942753216E-16,6.40667124022599));
#5057=CARTESIAN_POINT('Origin',(21.1848248598985,0.,-4.66385643997278));
#5058=CARTESIAN_POINT('',(21.1848248598985,-5.71157686089543E-16,4.66385643997278));
#5059=CARTESIAN_POINT('Origin',(21.1848248598985,0.,0.));
#5060=CARTESIAN_POINT('Origin',(20.4983944566926,0.,0.));
#5061=CARTESIAN_POINT('',(19.8119640534868,-5.71157686089543E-16,4.66385643997278));
#5062=CARTESIAN_POINT('Origin',(19.8119640534868,0.,0.));
#5063=CARTESIAN_POINT('',(20.4983944566926,-5.71157686089543E-16,4.66385643997278));
#5064=CARTESIAN_POINT('Origin',(19.8119640534868,0.,-3.44589712386029));
#5065=CARTESIAN_POINT('',(19.8119640534868,-4.22000688292658E-16,3.44589712386029));
#5066=CARTESIAN_POINT('Origin',(19.8119640534868,0.,0.));
#5067=CARTESIAN_POINT('Origin',(15.9443326090014,0.,0.));
#5068=CARTESIAN_POINT('',(15.9443326090014,-4.22000688292657E-16,3.44589712386029));
#5069=CARTESIAN_POINT('Origin',(11.0238490761438,0.,-6.89179424772059));
#5070=CARTESIAN_POINT('',(0.,0.,0.));
#5071=CARTESIAN_POINT('Origin',(88.3562164250559,0.,0.));
#5072=CARTESIAN_POINT('',(90.9367078804579,1.77561363837187,-0.0475422940951198));
#5073=CARTESIAN_POINT('',(90.790457845232,1.77561363837197,-0.0475422940912425));
#5074=CARTESIAN_POINT('',(88.3562164250559,1.77561363837197,-0.0475422940912398));
#5075=CARTESIAN_POINT('',(90.3790868290973,0.00149166109910448,1.77624937366552));
#5076=CARTESIAN_POINT('Ctrl Pts',(90.9367078804579,1.77561363837187,-0.0475422940950947));
#5077=CARTESIAN_POINT('Ctrl Pts',(90.9364406478333,1.7755088947135,-0.05145426914555));
#5078=CARTESIAN_POINT('Ctrl Pts',(90.9361741013816,1.77539122163591,-0.0553659470277124));
#5079=CARTESIAN_POINT('Ctrl Pts',(90.9354289302851,1.77502512697568,-0.0663299051595725));
#5080=CARTESIAN_POINT('Ctrl Pts',(90.9349519773079,1.77474761564714,-0.0733809392859071));
#5081=CARTESIAN_POINT('Ctrl Pts',(90.9338700479988,1.77401920580607,-0.0894508407210216));
#5082=CARTESIAN_POINT('Ctrl Pts',(90.9332665466041,1.7735415502998,-0.0984681352261746));
#5083=CARTESIAN_POINT('Ctrl Pts',(90.9313857021166,1.77182868231983,-0.126723255478906));
#5084=CARTESIAN_POINT('Ctrl Pts',(90.9301209560697,1.77034901257526,-0.145945574748464));
#5085=CARTESIAN_POINT('Ctrl Pts',(90.9271215763623,1.7660535158258,-0.191947670512226));
#5086=CARTESIAN_POINT('Ctrl Pts',(90.9253998762074,1.7629411144518,-0.218695472152004));
#5087=CARTESIAN_POINT('Ctrl Pts',(90.9185480272457,1.74797956202784,-0.325967674584511));
#5088=CARTESIAN_POINT('Ctrl Pts',(90.9135720397987,1.73121033391175,-0.405709252183148));
#5089=CARTESIAN_POINT('Ctrl Pts',(90.9019699944758,1.67970739744729,-0.587559898655641));
#5090=CARTESIAN_POINT('Ctrl Pts',(90.8953431282698,1.64104035264349,-0.688205369161317));
#5091=CARTESIAN_POINT('Ctrl Pts',(90.8868307636316,1.58265962080283,-0.806756158773526));
#5092=CARTESIAN_POINT('Ctrl Pts',(90.8852351222549,1.57135666021832,-0.828556049690737));
#5093=CARTESIAN_POINT('Ctrl Pts',(90.8826014014651,1.55214864891183,-0.863794774706981));
#5094=CARTESIAN_POINT('Ctrl Pts',(90.8815727556905,1.5445119213898,-0.877376623809287));
#5095=CARTESIAN_POINT('Ctrl Pts',(90.8797055013338,1.53041499760629,-0.901693362873107));
#5096=CARTESIAN_POINT('Ctrl Pts',(90.8788692159976,1.52401796437476,-0.912463816263084));
#5097=CARTESIAN_POINT('Ctrl Pts',(90.8770608598892,1.51001030365971,-0.935489734553268));
#5098=CARTESIAN_POINT('Ctrl Pts',(90.8760874939559,1.50236326652315,-0.947721876188245));
#5099=CARTESIAN_POINT('Ctrl Pts',(90.8733649913025,1.48068380974828,-0.981478314697449));
#5100=CARTESIAN_POINT('Ctrl Pts',(90.8716041266841,1.46633256015355,-1.0027925654589));
#5101=CARTESIAN_POINT('Ctrl Pts',(90.8640001035302,1.40299491096074,-1.09259264298843));
#5102=CARTESIAN_POINT('Ctrl Pts',(90.8579947681781,1.34964111770653,-1.15785089795823));
#5103=CARTESIAN_POINT('Ctrl Pts',(90.8426298158545,1.20429945138372,-1.31187150595062));
#5104=CARTESIAN_POINT('Ctrl Pts',(90.8331636770439,1.10698655422456,-1.39496453935183));
#5105=CARTESIAN_POINT('Ctrl Pts',(90.8225011795454,0.982406882686855,-1.48002751671084));
#5106=CARTESIAN_POINT('Ctrl Pts',(90.8208744920965,0.962947193885271,-1.49276172278426));
#5107=CARTESIAN_POINT('Ctrl Pts',(90.8186447573278,0.935566062419342,-1.50992127779915));
#5108=CARTESIAN_POINT('Ctrl Pts',(90.8180230580811,0.927853263265728,-1.51467305149509));
#5109=CARTESIAN_POINT('Ctrl Pts',(90.8169117880306,0.913919415775024,-1.52311117268993));
#5110=CARTESIAN_POINT('Ctrl Pts',(90.8164208879198,0.907711579817898,-1.52681892776984));
#5111=CARTESIAN_POINT('Ctrl Pts',(90.8154093083889,0.894806694745356,-1.53442009999958));
#5112=CARTESIAN_POINT('Ctrl Pts',(90.8148889836212,0.888106555159891,-1.53830777696759));
#5113=CARTESIAN_POINT('Ctrl Pts',(90.8135111430629,0.870205266059774,-1.54853884429454));
#5114=CARTESIAN_POINT('Ctrl Pts',(90.8126583732215,0.858959991189343,-1.5548046548435));
#5115=CARTESIAN_POINT('Ctrl Pts',(90.8082958618394,0.800639346221723,-1.58647472625119));
#5116=CARTESIAN_POINT('Ctrl Pts',(90.8048946921989,0.752497407587655,-1.60986777132373));
#5117=CARTESIAN_POINT('Ctrl Pts',(90.7907852954617,0.545390013993606,-1.69917981864387));
#5118=CARTESIAN_POINT('Ctrl Pts',(90.7805650191555,0.378360401570082,-1.74399212453831));
#5119=CARTESIAN_POINT('Ctrl Pts',(90.7678905896674,0.18291815532491,-1.76697964699746));
#5120=CARTESIAN_POINT('Ctrl Pts',(90.766283107693,0.158290967091757,-1.7693558145486));
#5121=CARTESIAN_POINT('Ctrl Pts',(90.7636332423648,0.118022107291155,-1.77239375459435));
#5122=CARTESIAN_POINT('Ctrl Pts',(90.7626004549225,0.102406663617898,-1.77336451084305));
#5123=CARTESIAN_POINT('Ctrl Pts',(90.7607277113767,0.0742484381325717,-1.77474185976951));
#5124=CARTESIAN_POINT('Ctrl Pts',(90.7598901137838,0.0617101773089686,-1.77522205358507));
#5125=CARTESIAN_POINT('Ctrl Pts',(90.7580811230724,0.0347573469733052,-1.77596841747888));
#5126=CARTESIAN_POINT('Ctrl Pts',(90.7571084574451,0.0203426008238719,-1.77619200828667));
#5127=CARTESIAN_POINT('Ctrl Pts',(90.7543939580964,-0.0196611554975341,
-1.77632549583768));
#5128=CARTESIAN_POINT('Ctrl Pts',(90.7526405406671,-0.0452470277500012,
-1.77585793796779));
#5129=CARTESIAN_POINT('Ctrl Pts',(90.7451082126153,-0.154032241144647,-1.77151760885236));
#5130=CARTESIAN_POINT('Ctrl Pts',(90.739170874313,-0.236903575661729,-1.76234894663126));
#5131=CARTESIAN_POINT('Ctrl Pts',(90.7242598777567,-0.439148955545672,-1.72544899074502));
#5132=CARTESIAN_POINT('Ctrl Pts',(90.7151928678592,-0.556890668247468,-1.69112371261827));
#5133=CARTESIAN_POINT('Ctrl Pts',(90.7044862299971,-0.696376849201785,-1.63429618824903));
#5134=CARTESIAN_POINT('Ctrl Pts',(90.7024975405662,-0.722324877688078,-1.62299468088015));
#5135=CARTESIAN_POINT('Ctrl Pts',(90.6997969830317,-0.757751871638434,-1.60654658113198));
#5136=CARTESIAN_POINT('Ctrl Pts',(90.6990577921756,-0.767469246832142,-1.6019272099874));
#5137=CARTESIAN_POINT('Ctrl Pts',(90.6978320942622,-0.783626006802249,-1.59406596531438));
#5138=CARTESIAN_POINT('Ctrl Pts',(90.6973427239503,-0.790088596149161,-1.5908727280353));
#5139=CARTESIAN_POINT('Ctrl Pts',(90.6963377104244,-0.803388887721289,-1.5841998652902));
#5140=CARTESIAN_POINT('Ctrl Pts',(90.6958223965398,-0.810223814011509,-1.58071512137936));
#5141=CARTESIAN_POINT('Ctrl Pts',(90.6944569908053,-0.828367329306277,-1.57131616269045));
#5142=CARTESIAN_POINT('Ctrl Pts',(90.6936116210907,-0.839635369012165,-1.56532405143173));
#5143=CARTESIAN_POINT('Ctrl Pts',(90.6892939826121,-0.897297787560878,-1.53385852329897));
#5144=CARTESIAN_POINT('Ctrl Pts',(90.6859293689884,-0.942605925081128,-1.50643968126981));
#5145=CARTESIAN_POINT('Ctrl Pts',(90.6723962832535,-1.12259627611808,-1.38621022416122));
#5146=CARTESIAN_POINT('Ctrl Pts',(90.6626870602337,-1.24537114954097,-1.27704934107327));
#5147=CARTESIAN_POINT('Ctrl Pts',(90.6500456738212,-1.37380638022623,-1.12645613364311));
#5148=CARTESIAN_POINT('Ctrl Pts',(90.6478226219318,-1.39536232499479,-1.09964136062491));
#5149=CARTESIAN_POINT('Ctrl Pts',(90.6445181375125,-1.42580205583846,-1.05943831812827));
#5150=CARTESIAN_POINT('Ctrl Pts',(90.6434611041254,-1.43530524041664,-1.04652753952237));
#5151=CARTESIAN_POINT('Ctrl Pts',(90.6415680174533,-1.45190194345323,-1.02332835565672));
#5152=CARTESIAN_POINT('Ctrl Pts',(90.6407347009393,-1.45906417564596,-1.01309026964812));
#5153=CARTESIAN_POINT('Ctrl Pts',(90.6389606136308,-1.47400566378672,-0.991244969840101));
#5154=CARTESIAN_POINT('Ctrl Pts',(90.6380188571002,-1.48175712458954,-0.979619870800271));
#5155=CARTESIAN_POINT('Ctrl Pts',(90.6354594795324,-1.50233343771649,-0.947957922257173));
#5156=CARTESIAN_POINT('Ctrl Pts',(90.6338321691614,-1.51489382192812,-0.927753519175028));
#5157=CARTESIAN_POINT('Ctrl Pts',(90.6301785787599,-1.54192939241401,-0.882251108812333));
#5158=CARTESIAN_POINT('Ctrl Pts',(90.6281454644399,-1.55619506279705,-0.856837223838339));
#5159=CARTESIAN_POINT('Ctrl Pts',(90.6214982588089,-1.60033899086924,-0.773454197305031));
#5160=CARTESIAN_POINT('Ctrl Pts',(90.6168074786084,-1.62764994047824,-0.714192200532683));
#5161=CARTESIAN_POINT('Ctrl Pts',(90.6050019226972,-1.68736670940282,-0.563281292074101));
#5162=CARTESIAN_POINT('Ctrl Pts',(90.5978372502738,-1.715630527162,-0.470217389575858));
#5163=CARTESIAN_POINT('Ctrl Pts',(90.5878271468518,-1.74502631577079,-0.334235186265452));
#5164=CARTESIAN_POINT('Ctrl Pts',(90.5848416840981,-1.7524458926945,-0.292854939791319));
#5165=CARTESIAN_POINT('Ctrl Pts',(90.5810695502963,-1.76013237667591,-0.239059905010199));
#5166=CARTESIAN_POINT('Ctrl Pts',(90.5802209201071,-1.76174704817757,-0.22685453779923));
#5167=CARTESIAN_POINT('Ctrl Pts',(90.578860302099,-1.76415135535286,-0.207102873126839));
#5168=CARTESIAN_POINT('Ctrl Pts',(90.5783441518275,-1.76501974263209,-0.199566826560699));
#5169=CARTESIAN_POINT('Ctrl Pts',(90.5773306912117,-1.76663865644254,-0.184679502025739));
#5170=CARTESIAN_POINT('Ctrl Pts',(90.5768332525516,-1.76739164093947,-0.177328658917269));
#5171=CARTESIAN_POINT('Ctrl Pts',(90.5755863520991,-1.769172932245,-0.158799270129472));
#5172=CARTESIAN_POINT('Ctrl Pts',(90.5748401425478,-1.77014120249121,-0.147615079978273));
#5173=CARTESIAN_POINT('Ctrl Pts',(90.5718371743613,-1.77363506255843,-0.102258514779939));
#5174=CARTESIAN_POINT('Ctrl Pts',(90.5696238404745,-1.77527781888608,-0.068023265765211));
#5175=CARTESIAN_POINT('Ctrl Pts',(90.5634622930758,-1.77711798315338,0.0287794297197061));
#5176=CARTESIAN_POINT('Ctrl Pts',(90.559593290057,-1.77500262495174,0.0913418981976327));
#5177=CARTESIAN_POINT('Ctrl Pts',(90.5473512532474,-1.75778691318612,0.289594850817781));
#5178=CARTESIAN_POINT('Ctrl Pts',(90.5390599267307,-1.73036340619092,0.42369608380026));
#5179=CARTESIAN_POINT('Ctrl Pts',(90.5286058814987,-1.67991461230748,0.577583099874535));
#5180=CARTESIAN_POINT('Ctrl Pts',(90.5269432945398,-1.67144328199262,0.601658200806042));
#5181=CARTESIAN_POINT('Ctrl Pts',(90.5243040799533,-1.65732118387112,0.639189483336105));
#5182=CARTESIAN_POINT('Ctrl Pts',(90.5233389493616,-1.6520180482435,0.652773352068889));
#5183=CARTESIAN_POINT('Ctrl Pts',(90.5216142649825,-1.64230019469282,0.676788292740844));
#5184=CARTESIAN_POINT('Ctrl Pts',(90.5208569756628,-1.63795177301964,0.687245445055579));
#5185=CARTESIAN_POINT('Ctrl Pts',(90.5190901271027,-1.62762026003468,0.711435684910198));
#5186=CARTESIAN_POINT('Ctrl Pts',(90.518078093155,-1.62156292498031,0.725135919063111));
#5187=CARTESIAN_POINT('Ctrl Pts',(90.5151428916477,-1.60359987427085,0.764413097628829));
#5188=CARTESIAN_POINT('Ctrl Pts',(90.5132050052202,-1.59125762523076,0.789784117986039));
#5189=CARTESIAN_POINT('Ctrl Pts',(90.5087230536394,-1.56163446014763,0.847162516906397));
#5190=CARTESIAN_POINT('Ctrl Pts',(90.5061666998465,-1.54396452489455,0.878953783391171));
#5191=CARTESIAN_POINT('Ctrl Pts',(90.4967276419374,-1.47591040084928,0.993003005017456));
#5192=CARTESIAN_POINT('Ctrl Pts',(90.4896806575694,-1.41982860034292,1.0716575807583));
#5193=CARTESIAN_POINT('Ctrl Pts',(90.4766256718245,-1.30459225405994,1.20825197639796));
#5194=CARTESIAN_POINT('Ctrl Pts',(90.4706357231352,-1.24722682831556,1.26738373712288));
#5195=CARTESIAN_POINT('Ctrl Pts',(90.4635911250846,-1.17242148549561,1.33447473370843));
#5196=CARTESIAN_POINT('Ctrl Pts',(90.4623272400515,-1.15869317950186,1.34641194810373));
#5197=CARTESIAN_POINT('Ctrl Pts',(90.4604673720094,-1.13799693689821,1.36385696084663));
#5198=CARTESIAN_POINT('Ctrl Pts',(90.4598608449729,-1.13116764329429,1.36952641786419));
#5199=CARTESIAN_POINT('Ctrl Pts',(90.4587698246762,-1.11873261545039,1.37969309531884));
#5200=CARTESIAN_POINT('Ctrl Pts',(90.4582841636812,-1.11314188310701,1.38420766252412));
#5201=CARTESIAN_POINT('Ctrl Pts',(90.4571831855773,-1.10034333783009,1.39441491318847));
#5202=CARTESIAN_POINT('Ctrl Pts',(90.456569361653,-1.09311858222134,1.4000857779059));
#5203=CARTESIAN_POINT('Ctrl Pts',(90.4546657645702,-1.0704465932619,1.41759902385506));
#5204=CARTESIAN_POINT('Ctrl Pts',(90.4533884615712,-1.05484792220282,1.42924414872662));
#5205=CARTESIAN_POINT('Ctrl Pts',(90.4465481035699,-0.969429811660141,1.49085226171763));
#5206=CARTESIAN_POINT('Ctrl Pts',(90.4412311971354,-0.896241933193827,1.53596492986674));
#5207=CARTESIAN_POINT('Ctrl Pts',(90.4291874646331,-0.723032100909454,1.62611686355231));
#5208=CARTESIAN_POINT('Ctrl Pts',(90.4224892885638,-0.62154285176125,1.66754722517513));
#5209=CARTESIAN_POINT('Ctrl Pts',(90.4131880519771,-0.482157299403821,1.70994340869914));
#5210=CARTESIAN_POINT('Ctrl Pts',(90.4108429667422,-0.447109704668306,1.71944024357985));
#5211=CARTESIAN_POINT('Ctrl Pts',(90.4073928178437,-0.395889829676749,1.73164740463657));
#5212=CARTESIAN_POINT('Ctrl Pts',(90.4063146914316,-0.379930978291518,1.7352186933647));
#5213=CARTESIAN_POINT('Ctrl Pts',(90.404382367012,-0.351427985210454,1.74118507508166));
#5214=CARTESIAN_POINT('Ctrl Pts',(90.4035309399273,-0.338902893809712,1.74366622627442));
#5215=CARTESIAN_POINT('Ctrl Pts',(90.401879394256,-0.314680080017998,1.74819378586932));
#5216=CARTESIAN_POINT('Ctrl Pts',(90.4010798972719,-0.302986414349454,1.75025834854431));
#5217=CARTESIAN_POINT('Ctrl Pts',(90.3993386860087,-0.277594124432116,1.75447936762318));
#5218=CARTESIAN_POINT('Ctrl Pts',(90.3983956820409,-0.263889269859646,1.7565929476446));
#5219=CARTESIAN_POINT('Ctrl Pts',(90.3953272929415,-0.219456873991419,1.76291366473226));
#5220=CARTESIAN_POINT('Ctrl Pts',(90.3931822805761,-0.188644984952052,1.76647637174408));
#5221=CARTESIAN_POINT('Ctrl Pts',(90.3872951384509,-0.10478676224065,1.77395376904623));
#5222=CARTESIAN_POINT('Ctrl Pts',(90.3835097511813,-0.0516363347368595,
1.77629526122296));
#5223=CARTESIAN_POINT('Ctrl Pts',(90.3796762924913,0.00153415989328701,
1.77624933746741));
#5224=CARTESIAN_POINT('',(90.3499141080351,0.430772083774147,1.72400118248596));
#5225=CARTESIAN_POINT('Ctrl Pts',(90.3499212718705,0.430397524873051,1.72331715974836));
#5226=CARTESIAN_POINT('Ctrl Pts',(90.354782198075,0.360606047738533,1.74074754326541));
#5227=CARTESIAN_POINT('Ctrl Pts',(90.3596431242794,0.289637073919477,1.75396322484711));
#5228=CARTESIAN_POINT('Ctrl Pts',(90.3645040504839,0.217984708007283,1.76282351061443));
#5229=CARTESIAN_POINT('Ctrl Pts',(90.3693649766884,0.146332342095089,1.77168379638175));
#5230=CARTESIAN_POINT('Ctrl Pts',(90.3742259028928,0.0739968663745415,1.77618848514627));
#5231=CARTESIAN_POINT('Ctrl Pts',(90.3790868290973,0.00149166109910448,
1.77624937366552));
#5232=CARTESIAN_POINT('',(90.3498698986825,-1.48890580190326,0.968619417293912));
#5233=CARTESIAN_POINT('Origin',(90.3498698986825,0.,0.));
#5234=CARTESIAN_POINT('Ctrl Pts',(90.3498698986825,-1.48890580190326,0.968619417293917));
#5235=CARTESIAN_POINT('Ctrl Pts',(90.3542650496983,-1.52457107695468,0.913796817207203));
#5236=CARTESIAN_POINT('Ctrl Pts',(90.3586602007142,-1.55723341380908,0.856958034254269));
#5237=CARTESIAN_POINT('Ctrl Pts',(90.36305535173,-1.58667231885172,0.798457898132208));
#5238=CARTESIAN_POINT('Ctrl Pts',(90.3674705710205,-1.61624564203603,0.739690650187431));
#5239=CARTESIAN_POINT('Ctrl Pts',(90.371885790311,-1.64256575033591,0.679247235760215));
#5240=CARTESIAN_POINT('Ctrl Pts',(90.3763010096014,-1.66545525170715,0.617513454963586));
#5241=CARTESIAN_POINT('Ctrl Pts',(90.3806927242746,-1.68822289979423,0.556108316709745));
#5242=CARTESIAN_POINT('Ctrl Pts',(90.3850844389477,-1.70759623302425,0.493426970910843));
#5243=CARTESIAN_POINT('Ctrl Pts',(90.3894761536209,-1.72344922018923,0.429868407689064));
#5244=CARTESIAN_POINT('Ctrl Pts',(90.3938679372515,-1.73930245627353,0.366308846487906));
#5245=CARTESIAN_POINT('Ctrl Pts',(90.3982597208822,-1.75163512245982,0.301872497983461));
#5246=CARTESIAN_POINT('Ctrl Pts',(90.4026515045129,-1.76037179242643,0.236970915787881));
#5247=CARTESIAN_POINT('Ctrl Pts',(90.4070446198946,-1.76911111167417,0.172049653034722));
#5248=CARTESIAN_POINT('Ctrl Pts',(90.4114377352763,-1.77425220553906,0.106663343536512));
#5249=CARTESIAN_POINT('Ctrl Pts',(90.415830850658,-1.77577143528477,0.0412295055351104));
#5250=CARTESIAN_POINT('Ctrl Pts',(90.420263330995,-1.77730427824246,-0.0247906589979149));
#5251=CARTESIAN_POINT('Ctrl Pts',(90.4246958113319,-1.7751500030428,-0.0908587202707488));
#5252=CARTESIAN_POINT('Ctrl Pts',(90.4291282916689,-1.76933800722062,-0.156547368884247));
#5253=CARTESIAN_POINT('Ctrl Pts',(90.4335309847615,-1.7635650692908,-0.221794575307162));
#5254=CARTESIAN_POINT('Ctrl Pts',(90.4379336778541,-1.754183558958,-0.286666991404655));
#5255=CARTESIAN_POINT('Ctrl Pts',(90.4423363709467,-1.74127406352506,-0.350754469957176));
#5256=CARTESIAN_POINT('Ctrl Pts',(90.4467837449058,-1.72823355567973,-0.415492342261526));
#5257=CARTESIAN_POINT('Ctrl Pts',(90.451231118865,-1.71159317016332,-0.479428777441116));
#5258=CARTESIAN_POINT('Ctrl Pts',(90.4556784928241,-1.69148746417727,-0.542157007730383));
#5259=CARTESIAN_POINT('Ctrl Pts',(90.4601258667833,-1.67138175819121,-0.604885238019651));
#5260=CARTESIAN_POINT('Ctrl Pts',(90.4645732407425,-1.64781096407574,-0.666404828878841));
#5261=CARTESIAN_POINT('Ctrl Pts',(90.4690206147016,-1.62095839669095,-0.726331837865526));
#5262=CARTESIAN_POINT('Ctrl Pts',(90.4732817188201,-1.59523049826715,-0.783748917504813));
#5263=CARTESIAN_POINT('Ctrl Pts',(90.4775428229385,-1.56638569702523,-0.839936213934016));
#5264=CARTESIAN_POINT('Ctrl Pts',(90.4818039270569,-1.53456308597654,-0.894527918881331));
#5265=CARTESIAN_POINT('Ctrl Pts',(90.4862359022096,-1.50146438255593,-0.951308760921983));
#5266=CARTESIAN_POINT('Ctrl Pts',(90.4906678773623,-1.46514408957627,-1.00636277571506));
#5267=CARTESIAN_POINT('Ctrl Pts',(90.4950998525149,-1.42581458344523,-1.05930016337906));
#5268=CARTESIAN_POINT('Ctrl Pts',(90.4993477343201,-1.38811872826863,-1.11003866215809));
#5269=CARTESIAN_POINT('Ctrl Pts',(90.5035956161253,-1.34765904649706,-1.15883242890056));
#5270=CARTESIAN_POINT('Ctrl Pts',(90.5078434979305,-1.3046685113476,-1.20536473235201));
#5271=CARTESIAN_POINT('Ctrl Pts',(90.5120883386773,-1.26170875312058,-1.25186372332924));
#5272=CARTESIAN_POINT('Ctrl Pts',(90.516333179424,-1.21622207966895,-1.29610408253071));
#5273=CARTESIAN_POINT('Ctrl Pts',(90.5205780201708,-1.16848166994252,-1.33780217129004));
#5274=CARTESIAN_POINT('Ctrl Pts',(90.5248214199474,-1.12075746636133,-1.37948610505391));
#5275=CARTESIAN_POINT('Ctrl Pts',(90.529064819724,-1.07078143086178,-1.4186291419559));
#5276=CARTESIAN_POINT('Ctrl Pts',(90.5333082195006,-1.01886197753949,-1.45498602509588));
#5277=CARTESIAN_POINT('Ctrl Pts',(90.5375517761135,-0.966940605271517,-1.49134425198815));
#5278=CARTESIAN_POINT('Ctrl Pts',(90.5417953327264,-0.913076095775772,-1.52491582865905));
#5279=CARTESIAN_POINT('Ctrl Pts',(90.5460388893393,-0.857606422015877,-1.55549840482629));
#5280=CARTESIAN_POINT('Ctrl Pts',(90.5502869934474,-0.802077305646338,-1.58611375400288));
#5281=CARTESIAN_POINT('Ctrl Pts',(90.5545350975556,-0.744940045311707,-1.61373346556902));
#5282=CARTESIAN_POINT('Ctrl Pts',(90.5587832016638,-0.686556629401138,-1.63820147024881));
#5283=CARTESIAN_POINT('Ctrl Pts',(90.5630340088166,-0.628136064453105,-1.66268504378164));
#5284=CARTESIAN_POINT('Ctrl Pts',(90.5672848159693,-0.56846825163121,-1.68401275130926));
#5285=CARTESIAN_POINT('Ctrl Pts',(90.5715356231221,-0.50793161955539,-1.70207800419248));
#5286=CARTESIAN_POINT('Ctrl Pts',(90.5757937716034,-0.44729043808791,-1.72017445655169));
#5287=CARTESIAN_POINT('Ctrl Pts',(90.5800519200847,-0.385777944191992,-1.73499710021916));
#5288=CARTESIAN_POINT('Ctrl Pts',(90.584310068566,-0.32378277377414,-1.74649041735336));
#5289=CARTESIAN_POINT('Ctrl Pts',(90.5855971559509,-0.305043830751616,-1.74996443982102));
#5290=CARTESIAN_POINT('Ctrl Pts',(90.5868842433359,-0.286260816369676,-1.75313464227076));
#5291=CARTESIAN_POINT('Ctrl Pts',(90.5881713307208,-0.267444501795399,-1.75600042738019));
#5292=CARTESIAN_POINT('Ctrl Pts',(90.5924735824778,-0.204548599478252,-1.76557967519693));
#5293=CARTESIAN_POINT('Ctrl Pts',(90.5967758342347,-0.141009940094459,-1.77179489134502));
#5294=CARTESIAN_POINT('Ctrl Pts',(90.6010780859917,-0.0772198733713044,
-1.77457069559275));
#5295=CARTESIAN_POINT('Ctrl Pts',(90.6055049176896,-0.0115826430720942,
-1.7774268785697));
#5296=CARTESIAN_POINT('Ctrl Pts',(90.6099317493874,0.0543202676253199,-1.77664118668768));
#5297=CARTESIAN_POINT('Ctrl Pts',(90.6143585810852,0.12005235508134,-1.77218833495185));
#5298=CARTESIAN_POINT('Ctrl Pts',(90.6186489176737,0.183757686365544,-1.76787278061653));
#5299=CARTESIAN_POINT('Ctrl Pts',(90.6229392542622,0.247302032647212,-1.76011297008372));
#5300=CARTESIAN_POINT('Ctrl Pts',(90.6272295908507,0.310286434006175,-1.7489386471148));
#5301=CARTESIAN_POINT('Ctrl Pts',(90.6315172607396,0.37323168681021,-1.73777126965281));
#5302=CARTESIAN_POINT('Ctrl Pts',(90.6358049306285,0.435617190748632,-1.72319367647727));
#5303=CARTESIAN_POINT('Ctrl Pts',(90.6400926005174,0.497050741105725,-1.70528725535209));
#5304=CARTESIAN_POINT('Ctrl Pts',(90.644379141861,0.558468121714196,-1.68738554732465));
#5305=CARTESIAN_POINT('Ctrl Pts',(90.6486656832046,0.618933563499767,-1.66615689140698));
#5306=CARTESIAN_POINT('Ctrl Pts',(90.6529522245482,0.678068587108382,-1.64173294225244));
#5307=CARTESIAN_POINT('Ctrl Pts',(90.6572391736718,0.737209236249965,-1.6173066696401));
#5308=CARTESIAN_POINT('Ctrl Pts',(90.6615261227954,0.795018752432631,-1.58968469543067));
#5309=CARTESIAN_POINT('Ctrl Pts',(90.665813071919,0.851139090974467,-1.55904660299657));
#5310=CARTESIAN_POINT('Ctrl Pts',(90.6701046721401,0.907320316911708,-1.52837526996384));
#5311=CARTESIAN_POINT('Ctrl Pts',(90.6743962723612,0.961808267680585,-1.49468153315526));
#5312=CARTESIAN_POINT('Ctrl Pts',(90.6786878725823,1.01427103013557,-1.45819009046411));
#5313=CARTESIAN_POINT('Ctrl Pts',(90.6829822939531,1.06676827979854,-1.42167465955894));
#5314=CARTESIAN_POINT('Ctrl Pts',(90.687276715324,1.11723729617056,-1.38235817295531));
#5315=CARTESIAN_POINT('Ctrl Pts',(90.6915711366948,1.16537893228083,-1.34050587715832));
#5316=CARTESIAN_POINT('Ctrl Pts',(90.6958726801322,1.21360040870171,-1.29858417158289));
#5317=CARTESIAN_POINT('Ctrl Pts',(90.7001742235696,1.25948644666761,-1.25411861877814));
#5318=CARTESIAN_POINT('Ctrl Pts',(90.704475767007,1.3027753085361,-1.20741068322616));
#5319=CARTESIAN_POINT('Ctrl Pts',(90.705424526918,1.31232321554433,-1.19710865619317));
#5320=CARTESIAN_POINT('Ctrl Pts',(90.7063732868289,1.32174493585239,-1.18669766337584));
#5321=CARTESIAN_POINT('Ctrl Pts',(90.7073220467399,1.33103793858093,-1.1761811376477));
#5322=CARTESIAN_POINT('Ctrl Pts',(90.7116269592798,1.37320410044859,-1.12846335050273));
#5323=CARTESIAN_POINT('Ctrl Pts',(90.7159318718197,1.41288366859533,-1.0783816722617));
#5324=CARTESIAN_POINT('Ctrl Pts',(90.7202367843596,1.44980187306361,-1.02622540962561));
#5325=CARTESIAN_POINT('Ctrl Pts',(90.7245356918203,1.48666857898457,-0.974141901658876));
#5326=CARTESIAN_POINT('Ctrl Pts',(90.7288345992809,1.52078127230915,-0.919989954391084));
#5327=CARTESIAN_POINT('Ctrl Pts',(90.7331335067416,1.55190447100271,-0.8640929205715));
#5328=CARTESIAN_POINT('Ctrl Pts',(90.7374279508293,1.58299535580106,-0.808253922267861));
#5329=CARTESIAN_POINT('Ctrl Pts',(90.7417223949169,1.61110266111203,-0.750673868712587));
#5330=CARTESIAN_POINT('Ctrl Pts',(90.7460168390046,1.63603450473893,-0.691704533600605));
#5331=CARTESIAN_POINT('Ctrl Pts',(90.7503089529768,1.66095282063736,-0.63276719456425));
#5332=CARTESIAN_POINT('Ctrl Pts',(90.7546010669491,1.68269889395222,-0.57244252918758));
#5333=CARTESIAN_POINT('Ctrl Pts',(90.7588931809213,1.70112787033456,-0.511104716541551));
#5334=CARTESIAN_POINT('Ctrl Pts',(90.7631839204141,1.71955094513826,-0.44978654632802));
#5335=CARTESIAN_POINT('Ctrl Pts',(90.767474659907,1.73465889208006,-0.387456354892826));
#5336=CARTESIAN_POINT('Ctrl Pts',(90.7717653993998,1.74635655767869,-0.32450398449422));
#5337=CARTESIAN_POINT('Ctrl Pts',(90.776057765654,1.75805865824954,-0.261527746768321));
#5338=CARTESIAN_POINT('Ctrl Pts',(90.7803501319082,1.766347806312,-0.197929353333886));
#5339=CARTESIAN_POINT('Ctrl Pts',(90.7846424981625,1.77118015857365,-0.134107823690546));
#5340=CARTESIAN_POINT('Ctrl Pts',(90.7865809471856,1.7733624673438,-0.105285776719741));
#5341=CARTESIAN_POINT('Ctrl Pts',(90.7885193962088,1.77484047957058,-0.0764182946841652));
#5342=CARTESIAN_POINT('Ctrl Pts',(90.790457845232,1.77561363837197,-0.0475422940912425));
#5343=CARTESIAN_POINT('Origin',(88.3562164250559,0.,0.));
#5344=CARTESIAN_POINT('',(91.6892085678292,1.77561362793331,-0.0475426839535425));
#5345=CARTESIAN_POINT('',(91.5405159974736,1.77561363837197,-0.0475422940912406));
#5346=CARTESIAN_POINT('',(88.3562164250559,1.77561363837197,-0.0475422940912398));
#5347=CARTESIAN_POINT('Ctrl Pts',(91.6892085678292,1.77561362793331,-0.0475426839535299));
#5348=CARTESIAN_POINT('Ctrl Pts',(91.68325628541,1.77340527983042,-0.130019579674131));
#5349=CARTESIAN_POINT('Ctrl Pts',(91.6771948219063,1.76545186668815,-0.212286424862139));
#5350=CARTESIAN_POINT('Ctrl Pts',(91.6656640609989,1.739318000267,-0.368140712732106));
#5351=CARTESIAN_POINT('Ctrl Pts',(91.6602047775528,1.72211467929499,-0.441676596123442));
#5352=CARTESIAN_POINT('Ctrl Pts',(91.6539885632293,1.69628166439824,-0.527147058730273));
#5353=CARTESIAN_POINT('Ctrl Pts',(91.6530325290953,1.69212377798698,-0.540344941896463));
#5354=CARTESIAN_POINT('Ctrl Pts',(91.6515411317898,1.68533810343189,-0.56103704525579));
#5355=CARTESIAN_POINT('Ctrl Pts',(91.6510001825116,1.68281366442813,-0.56856421453817));
#5356=CARTESIAN_POINT('Ctrl Pts',(91.6499745130515,1.67790451646542,-0.582882748657257));
#5357=CARTESIAN_POINT('Ctrl Pts',(91.6494893232398,1.67552889504532,-0.589676851045445));
#5358=CARTESIAN_POINT('Ctrl Pts',(91.6483177900537,1.66966431465331,-0.606127507070891));
#5359=CARTESIAN_POINT('Ctrl Pts',(91.6476339089797,1.66613273688137,-0.615768783062606));
#5360=CARTESIAN_POINT('Ctrl Pts',(91.64566887427,1.65567799621406,-0.643561826727751));
#5361=CARTESIAN_POINT('Ctrl Pts',(91.6443992182078,1.64854017658055,-0.661631930473293));
#5362=CARTESIAN_POINT('Ctrl Pts',(91.6347123104552,1.59124515305282,-0.799992338117911));
#5363=CARTESIAN_POINT('Ctrl Pts',(91.6268719473405,1.52827686563687,-0.914563967965044));
#5364=CARTESIAN_POINT('Ctrl Pts',(91.6136132141823,1.40461194741173,-1.09055469943526));
#5365=CARTESIAN_POINT('Ctrl Pts',(91.6083298694113,1.35100106874289,-1.15630360631929));
#5366=CARTESIAN_POINT('Ctrl Pts',(91.6011996568442,1.27524070565146,-1.23672511068899));
#5367=CARTESIAN_POINT('Ctrl Pts',(91.5995214372892,1.2571690836017,-1.2550910891414));
#5368=CARTESIAN_POINT('Ctrl Pts',(91.5968758150981,1.22835895390123,-1.2831238175237));
#5369=CARTESIAN_POINT('Ctrl Pts',(91.5959204085836,1.21789069629355,-1.29306406720859));
#5370=CARTESIAN_POINT('Ctrl Pts',(91.5941261064355,1.19812009984183,-1.31138438766517));
#5371=CARTESIAN_POINT('Ctrl Pts',(91.5932886316958,1.18884800960429,-1.31979588651493));
#5372=CARTESIAN_POINT('Ctrl Pts',(91.5914015343876,1.16786152965186,-1.33843389769051));
#5373=CARTESIAN_POINT('Ctrl Pts',(91.5903497251235,1.15610032891292,-1.3486058925982));
#5374=CARTESIAN_POINT('Ctrl Pts',(91.5876268503027,1.12549897368901,-1.37437781477037));
#5375=CARTESIAN_POINT('Ctrl Pts',(91.5859465971801,1.10646794060709,-1.38974490836504));
#5376=CARTESIAN_POINT('Ctrl Pts',(91.5764062045671,0.997632662000477,-1.47397397833268));
#5377=CARTESIAN_POINT('Ctrl Pts',(91.5682329767863,0.901739363217165,-1.53451244803781));
#5378=CARTESIAN_POINT('Ctrl Pts',(91.554322965559,0.731846480293256,-1.62031628804731));
#5379=CARTESIAN_POINT('Ctrl Pts',(91.5486579448799,0.660736790177042,-1.65059139542308));
#5380=CARTESIAN_POINT('Ctrl Pts',(91.5412435054073,0.563179575514897,-1.68480800715479));
#5381=CARTESIAN_POINT('Ctrl Pts',(91.5393821972104,0.538288791631596,-1.69292485842697));
#5382=CARTESIAN_POINT('Ctrl Pts',(91.5362184024868,0.495153533447352,-1.70594355812178));
#5383=CARTESIAN_POINT('Ctrl Pts',(91.5349050294414,0.476993896868415,-1.71110997272856));
#5384=CARTESIAN_POINT('Ctrl Pts',(91.5329908063195,0.45010301649039,-1.71829902345869));
#5385=CARTESIAN_POINT('Ctrl Pts',(91.5323783561629,0.441433967087397,-1.72054651808009));
#5386=CARTESIAN_POINT('Ctrl Pts',(91.5312899581227,0.425904048984359,-1.7244476216172));
#5387=CARTESIAN_POINT('Ctrl Pts',(91.5308126637137,0.419049919768289,-1.72612601749346));
#5388=CARTESIAN_POINT('Ctrl Pts',(91.5297477268693,0.403658645439486,-1.72979785149007));
#5389=CARTESIAN_POINT('Ctrl Pts',(91.5291613398985,0.395116552877595,-1.73176898771762));
#5390=CARTESIAN_POINT('Ctrl Pts',(91.5273891262743,0.369108930696934,-1.73756793820439));
#5391=CARTESIAN_POINT('Ctrl Pts',(91.5262139131143,0.351599288526059,-1.74119549246946));
#5392=CARTESIAN_POINT('Ctrl Pts',(91.5187779355657,0.239367849530657,-1.76268486340317));
#5393=CARTESIAN_POINT('Ctrl Pts',(91.5128506571035,0.143367824799995,-1.77307789274259));
#5394=CARTESIAN_POINT('Ctrl Pts',(91.5039892872169,-0.000898945261336359,
-1.77689562584708));
#5395=CARTESIAN_POINT('Ctrl Pts',(91.5010545382994,-0.0488175700636594,
-1.77622510462011));
#5396=CARTESIAN_POINT('Ctrl Pts',(91.4946268280648,-0.152664113404289,-1.77056619554675));
#5397=CARTESIAN_POINT('Ctrl Pts',(91.4911275415671,-0.208498793042176,-1.76486219064826));
#5398=CARTESIAN_POINT('Ctrl Pts',(91.4851029702985,-0.302123060112933,-1.75079252383094));
#5399=CARTESIAN_POINT('Ctrl Pts',(91.4826165786719,-0.340079450461037,-1.74381720044289));
#5400=CARTESIAN_POINT('Ctrl Pts',(91.4789925820975,-0.39418470360664,-1.73204054912488));
#5401=CARTESIAN_POINT('Ctrl Pts',(91.4778864894195,-0.410540879112052,-1.72823673114892));
#5402=CARTESIAN_POINT('Ctrl Pts',(91.4759336992656,-0.439124984767491,-1.72116050231054));
#5403=CARTESIAN_POINT('Ctrl Pts',(91.4750902738271,-0.451376621301081,-1.71798817181518));
#5404=CARTESIAN_POINT('Ctrl Pts',(91.4733227598521,-0.476849105852667,-1.7111012713601));
#5405=CARTESIAN_POINT('Ctrl Pts',(91.4723979754407,-0.490062823043254,-1.70736376956547));
#5406=CARTESIAN_POINT('Ctrl Pts',(91.4699522123687,-0.524702023403014,-1.69713083162884));
#5407=CARTESIAN_POINT('Ctrl Pts',(91.4684231114339,-0.546049749338592,-1.69038305253282));
#5408=CARTESIAN_POINT('Ctrl Pts',(91.4598472669505,-0.664021746462519,-1.65062553606843));
#5409=CARTESIAN_POINT('Ctrl Pts',(91.4525425847481,-0.757772088670623,-1.6097405652619));
#5410=CARTESIAN_POINT('Ctrl Pts',(91.4395751305044,-0.914278512007832,-1.52477414275634));
#5411=CARTESIAN_POINT('Ctrl Pts',(91.4339870529958,-0.978680957397881,-1.48425907131499));
#5412=CARTESIAN_POINT('Ctrl Pts',(91.4243598080906,-1.08629701772805,-1.40650081682382));
#5413=CARTESIAN_POINT('Ctrl Pts',(91.4202933304705,-1.13068906222673,-1.37106867932037));
#5414=CARTESIAN_POINT('Ctrl Pts',(91.41544047149,-1.18310655990328,-1.32495023662403));
#5415=CARTESIAN_POINT('Ctrl Pts',(91.4145402132914,-1.19280635572832,-1.31622463301532));
#5416=CARTESIAN_POINT('Ctrl Pts',(91.4131158605141,-1.20812727861732,-1.30213397460057));
#5417=CARTESIAN_POINT('Ctrl Pts',(91.4125869544873,-1.21381065304967,-1.29683773600981));
#5418=CARTESIAN_POINT('Ctrl Pts',(91.4115739097267,-1.22468864055343,-1.28656656402832));
#5419=CARTESIAN_POINT('Ctrl Pts',(91.4110894104585,-1.2298880377113,-1.28159713121034));
#5420=CARTESIAN_POINT('Ctrl Pts',(91.4100081510242,-1.24148061797128,-1.27038176044984));
#5421=CARTESIAN_POINT('Ctrl Pts',(91.409412680503,-1.24785722614641,-1.2641187814425));
#5422=CARTESIAN_POINT('Ctrl Pts',(91.4073273020998,-1.27014853022522,-1.24189165564753));
#5423=CARTESIAN_POINT('Ctrl Pts',(91.405855622513,-1.28580708547034,-1.2256722342066));
#5424=CARTESIAN_POINT('Ctrl Pts',(91.396110810024,-1.38860760748972,-1.11505043636696));
#5425=CARTESIAN_POINT('Ctrl Pts',(91.3883795158571,-1.46560417354145,-1.01172173940859));
#5426=CARTESIAN_POINT('Ctrl Pts',(91.3752548001773,-1.57359407653429,-0.828244374402557));
#5427=CARTESIAN_POINT('Ctrl Pts',(91.3699915110453,-1.61116098671449,-0.752558965538474));
#5428=CARTESIAN_POINT('Ctrl Pts',(91.3628857738388,-1.65296970274245,-0.65070469174771));
#5429=CARTESIAN_POINT('Ctrl Pts',(91.3612105498061,-1.6622170174491,-0.626705601985232));
#5430=CARTESIAN_POINT('Ctrl Pts',(91.3585686509802,-1.67583282533875,-0.588945235015135));
#5431=CARTESIAN_POINT('Ctrl Pts',(91.357613918196,-1.68056032492367,-0.575316540664702));
#5432=CARTESIAN_POINT('Ctrl Pts',(91.3558203040742,-1.6890794477124,-0.549755761445475));
#5433=CARTESIAN_POINT('Ctrl Pts',(91.3549828359578,-1.69291194881462,-0.537838170486027));
#5434=CARTESIAN_POINT('Ctrl Pts',(91.3530949901467,-1.70122495963668,-0.51101842276115));
#5435=CARTESIAN_POINT('Ctrl Pts',(91.3520424163737,-1.70563620612524,-0.496096056346474));
#5436=CARTESIAN_POINT('Ctrl Pts',(91.3493159769002,-1.71648671685574,-0.457534308563045));
#5437=CARTESIAN_POINT('Ctrl Pts',(91.3476328807635,-1.72263377343176,-0.433816863644595));
#5438=CARTESIAN_POINT('Ctrl Pts',(91.3382509220641,-1.75386926627506,-0.30214259620563));
#5439=CARTESIAN_POINT('Ctrl Pts',(91.3302531026308,-1.76929733532401,-0.192164098984426));
#5440=CARTESIAN_POINT('Ctrl Pts',(91.3163927829745,-1.77799963710245,-0.00266316402731915));
#5441=CARTESIAN_POINT('Ctrl Pts',(91.3105997154047,-1.77636341355964,0.0763133267285429));
#5442=CARTESIAN_POINT('Ctrl Pts',(91.3030385347111,-1.76717134824712,0.181303064497504));
#5443=CARTESIAN_POINT('Ctrl Pts',(91.3011548010791,-1.76427178061678,0.207630941515872));
#5444=CARTESIAN_POINT('Ctrl Pts',(91.297957258132,-1.75827715092089,0.252760941122569));
#5445=CARTESIAN_POINT('Ctrl Pts',(91.2966322705087,-1.75546643206794,0.271595860918295));
#5446=CARTESIAN_POINT('Ctrl Pts',(91.2947045605403,-1.75088434100287,0.299247087075983));
#5447=CARTESIAN_POINT('Ctrl Pts',(91.2940900109151,-1.74934816937235,0.308100285283694));
#5448=CARTESIAN_POINT('Ctrl Pts',(91.2929994972425,-1.74648570135877,0.32388509355939));
#5449=CARTESIAN_POINT('Ctrl Pts',(91.2925221614057,-1.74518520717268,0.330820882871658));
#5450=CARTESIAN_POINT('Ctrl Pts',(91.2914591104128,-1.7421820362496,0.346326650217968));
#5451=CARTESIAN_POINT('Ctrl Pts',(91.2908746267797,-1.74045742961265,0.35489201151041));
#5452=CARTESIAN_POINT('Ctrl Pts',(91.2891141085383,-1.73504183467548,0.380799488248176));
#5453=CARTESIAN_POINT('Ctrl Pts',(91.2879484855765,-1.73115420626327,0.398099976343473));
#5454=CARTESIAN_POINT('Ctrl Pts',(91.2781570305158,-1.69597973471441,0.544357433338902));
#5455=CARTESIAN_POINT('Ctrl Pts',(91.2701702780981,-1.65058753120124,0.669509519818571));
#5456=CARTESIAN_POINT('Ctrl Pts',(91.2566102990108,-1.55285658995098,0.866802171358049));
#5457=CARTESIAN_POINT('Ctrl Pts',(91.251167339358,-1.50831575611698,0.942173376839766));
#5458=CARTESIAN_POINT('Ctrl Pts',(91.2438426260323,-1.44349520068649,1.0354073445338));
#5459=CARTESIAN_POINT('Ctrl Pts',(91.2421412793614,-1.42810910883382,1.05652781427212));
#5460=CARTESIAN_POINT('Ctrl Pts',(91.2394673092088,-1.40346267234034,1.08883752137705));
#5461=CARTESIAN_POINT('Ctrl Pts',(91.2385071174246,-1.39452112575662,1.10026607210096));
#5462=CARTESIAN_POINT('Ctrl Pts',(91.2367084825461,-1.37760998147121,1.12134356083809));
#5463=CARTESIAN_POINT('Ctrl Pts',(91.2358715214746,-1.36967644338061,1.13102036635003));
#5464=CARTESIAN_POINT('Ctrl Pts',(91.2339917010964,-1.3517194055667,1.15245713955055));
#5465=CARTESIAN_POINT('Ctrl Pts',(91.2329467312469,-1.34164346415074,1.16417163624273));
#5466=CARTESIAN_POINT('Ctrl Pts',(91.2302541952085,-1.31545002736335,1.19383294355072));
#5467=CARTESIAN_POINT('Ctrl Pts',(91.2285977859649,-1.29911790318704,1.21158509640262));
#5468=CARTESIAN_POINT('Ctrl Pts',(91.2183200611899,-1.19649004726787,1.31867477192972));
#5469=CARTESIAN_POINT('Ctrl Pts',(91.2093131842151,-1.10139521766226,1.39907468922928));
#5470=CARTESIAN_POINT('Ctrl Pts',(91.1951495050721,-0.941240329206732,1.50796584707608));
#5471=CARTESIAN_POINT('Ctrl Pts',(91.1900634476284,-0.881519629631283,1.54363804668006));
#5472=CARTESIAN_POINT('Ctrl Pts',(91.1824798015324,-0.787545995094066,1.59253327175776));
#5473=CARTESIAN_POINT('Ctrl Pts',(91.179904593186,-0.754720059903905,1.60834976797192));
#5474=CARTESIAN_POINT('Ctrl Pts',(91.1765889126055,-0.710972525575328,1.6277939220882));
#5475=CARTESIAN_POINT('Ctrl Pts',(91.1758016599338,-0.700471632386018,1.63234018958223));
#5476=CARTESIAN_POINT('Ctrl Pts',(91.1745133950152,-0.683087585080062,1.63966780340691));
#5477=CARTESIAN_POINT('Ctrl Pts',(91.1740090067544,-0.676229775229471,1.64250797618951));
#5478=CARTESIAN_POINT('Ctrl Pts',(91.1729960307621,-0.662348589476972,1.6481552139936));
#5479=CARTESIAN_POINT('Ctrl Pts',(91.1724875448238,-0.655324717666835,1.65096056379733));
#5480=CARTESIAN_POINT('Ctrl Pts',(91.1711728210498,-0.63702540028215,1.65813416546171));
#5481=CARTESIAN_POINT('Ctrl Pts',(91.1703706161617,-0.625722668726462,1.6624323845356));
#5482=CARTESIAN_POINT('Ctrl Pts',(91.1669913450675,-0.57757432162533,1.68018166383017));
#5483=CARTESIAN_POINT('Ctrl Pts',(91.1644712002435,-0.540329687436431,1.69252676885963));
#5484=CARTESIAN_POINT('Ctrl Pts',(91.1549497168399,-0.395966428544315,1.73512521561807));
#5485=CARTESIAN_POINT('Ctrl Pts',(91.1482288337121,-0.286498786355872,1.75652235241753));
#5486=CARTESIAN_POINT('Ctrl Pts',(91.1377540351192,-0.117647347094808,1.773310901848));
#5487=CARTESIAN_POINT('Ctrl Pts',(91.1341183055209,-0.0593063493967736,
1.7762191493932));
#5488=CARTESIAN_POINT('Ctrl Pts',(91.1279426759111,0.0378385514972737,1.77627008327119));
#5489=CARTESIAN_POINT('Ctrl Pts',(91.1254469392346,0.0765962020687426,1.77502108118855));
#5490=CARTESIAN_POINT('Ctrl Pts',(91.1218934589584,0.130831531399746,1.77149373431687));
#5491=CARTESIAN_POINT('Ctrl Pts',(91.1208684531434,0.146368804344909,1.77027768668389));
#5492=CARTESIAN_POINT('Ctrl Pts',(91.1189885391545,0.174655352231179,1.76768887241048));
#5493=CARTESIAN_POINT('Ctrl Pts',(91.1181357491288,0.187409717095556,1.766382185413));
#5494=CARTESIAN_POINT('Ctrl Pts',(91.1163992235073,0.213217444564372,1.76345552157812));
#5495=CARTESIAN_POINT('Ctrl Pts',(91.1155153136268,0.226269170032844,1.76182839736807));
#5496=CARTESIAN_POINT('Ctrl Pts',(91.1133044939307,0.258695953653458,1.75741957744828));
#5497=CARTESIAN_POINT('Ctrl Pts',(91.1119721298375,0.27804496306384,1.75446234288203));
#5498=CARTESIAN_POINT('Ctrl Pts',(91.1065089780794,0.35657188779343,1.74112895975894));
#5499=CARTESIAN_POINT('Ctrl Pts',(91.1022953651592,0.415248285640318,1.7280743590951));
#5500=CARTESIAN_POINT('Ctrl Pts',(91.0903970120789,0.5758756093973,1.68368372478917));
#5501=CARTESIAN_POINT('Ctrl Pts',(91.0825617078658,0.675835764470835,1.64610632770786));
#5502=CARTESIAN_POINT('Ctrl Pts',(91.0695174860263,0.836954003363458,1.56837586327051));
#5503=CARTESIAN_POINT('Ctrl Pts',(91.0642904728375,0.900120941813972,1.53299687225567));
#5504=CARTESIAN_POINT('Ctrl Pts',(91.0582809446137,0.972700704378237,1.48630827231153));
#5505=CARTESIAN_POINT('Ctrl Pts',(91.0573161886683,0.98435225478397,1.4786174656265));
#5506=CARTESIAN_POINT('Ctrl Pts',(91.0558143004754,1.00250830764549,1.46632350107263));
#5507=CARTESIAN_POINT('Ctrl Pts',(91.0552714575822,1.00907429237472,1.46181277714816));
#5508=CARTESIAN_POINT('Ctrl Pts',(91.0542448711953,1.02150251479465,1.45315114961383));
#5509=CARTESIAN_POINT('Ctrl Pts',(91.0537606301867,1.02737018147873,1.44900868295922));
#5510=CARTESIAN_POINT('Ctrl Pts',(91.0525947347182,1.04150636499295,1.4388997585303));
#5511=CARTESIAN_POINT('Ctrl Pts',(91.0519154884229,1.04974908386172,1.43289737830857));
#5512=CARTESIAN_POINT('Ctrl Pts',(91.049490915183,1.07917481155081,1.41107923696332));
#5513=CARTESIAN_POINT('Ctrl Pts',(91.0477708046864,1.10005695092557,1.39486120083402));
#5514=CARTESIAN_POINT('Ctrl Pts',(91.0433798112992,1.15310357586009,1.35173011637927));
#5515=CARTESIAN_POINT('Ctrl Pts',(91.0407437027549,1.18469194591766,1.32413277723071));
#5516=CARTESIAN_POINT('Ctrl Pts',(91.033182620921,1.27335849177491,1.2409531821744));
#5517=CARTESIAN_POINT('Ctrl Pts',(91.0283364725427,1.32771218119164,1.18261899326054));
#5518=CARTESIAN_POINT('Ctrl Pts',(91.0176851014514,1.43681503705992,1.04848629623619));
#5519=CARTESIAN_POINT('Ctrl Pts',(91.0118703603176,1.48986548204182,0.971626809387183));
#5520=CARTESIAN_POINT('Ctrl Pts',(91.0043853027762,1.54776151583363,0.871774298212982));
#5521=CARTESIAN_POINT('Ctrl Pts',(91.0029349227798,1.55852746200069,0.852377976876884));
#5522=CARTESIAN_POINT('Ctrl Pts',(91.0005690621447,1.57534170156359,0.820700787354758));
#5523=CARTESIAN_POINT('Ctrl Pts',(90.9996616588206,1.58161642527279,0.808542345587602));
#5524=CARTESIAN_POINT('Ctrl Pts',(90.9979051086482,1.59342496061709,0.784997579750812));
#5525=CARTESIAN_POINT('Ctrl Pts',(90.9970567294771,1.59897874729834,0.773622166591484));
#5526=CARTESIAN_POINT('Ctrl Pts',(90.9950677135531,1.61164926206272,0.746950677830628));
#5527=CARTESIAN_POINT('Ctrl Pts',(90.9939238577632,1.61867049308735,0.731610866155257));
#5528=CARTESIAN_POINT('Ctrl Pts',(90.99010256062,1.64124382480983,0.680377050511052));
#5529=CARTESIAN_POINT('Ctrl Pts',(90.9873929470631,1.65582772611047,0.644071695454346));
#5530=CARTESIAN_POINT('Ctrl Pts',(90.9806271430366,1.68877199748613,0.553524910304817));
#5531=CARTESIAN_POINT('Ctrl Pts',(90.9765320167168,1.70573012229351,0.498823001959849));
#5532=CARTESIAN_POINT('Ctrl Pts',(90.9696910017619,1.72931567533396,0.407331467129618));
#5533=CARTESIAN_POINT('Ctrl Pts',(90.9669753030179,1.73747712635044,0.370978061596516));
#5534=CARTESIAN_POINT('Ctrl Pts',(90.9565242822811,1.76439780659845,0.230537233790908));
#5535=CARTESIAN_POINT('Ctrl Pts',(90.9487490797319,1.77499312743169,0.125100087455849));
#5536=CARTESIAN_POINT('Ctrl Pts',(90.9401102254816,1.77633543066197,0.00182430299203653));
#5537=CARTESIAN_POINT('Ctrl Pts',(90.9388935730831,1.7762670550413,-0.015693861606117));
#5538=CARTESIAN_POINT('Ctrl Pts',(90.9373616027383,1.7758501855836,-0.0379870968353825));
#5539=CARTESIAN_POINT('Ctrl Pts',(90.9370342299329,1.77574155328481,-0.042764917060308));
#5540=CARTESIAN_POINT('Ctrl Pts',(90.9367078804579,1.77561363837187,-0.0475422940950947));
#5541=CARTESIAN_POINT('',(90.9812164249928,0.00152582238372352,1.77624934464901));
#5542=CARTESIAN_POINT('Ctrl Pts',(90.790457845232,1.77561363837197,-0.0475422940912425));
#5543=CARTESIAN_POINT('Ctrl Pts',(90.7947551663863,1.77732764355503,0.0164725170880728));
#5544=CARTESIAN_POINT('Ctrl Pts',(90.7990524875405,1.77557414327281,0.0805287757352375));
#5545=CARTESIAN_POINT('Ctrl Pts',(90.8033498086948,1.7703849040683,0.144226744909051));
#5546=CARTESIAN_POINT('Ctrl Pts',(90.807655136144,1.76518599684554,0.208043389114973));
#5547=CARTESIAN_POINT('Ctrl Pts',(90.8119604635933,1.75653863148026,0.271499911855457));
#5548=CARTESIAN_POINT('Ctrl Pts',(90.8162657910424,1.7445262204379,0.334204022574007));
#5549=CARTESIAN_POINT('Ctrl Pts',(90.819668114948,1.735033304107,0.383756512457684));
#5550=CARTESIAN_POINT('Ctrl Pts',(90.8230704388535,1.72343993306419,0.43283922549068));
#5551=CARTESIAN_POINT('Ctrl Pts',(90.826472762759,1.70980912878435,0.481265836753137));
#5552=CARTESIAN_POINT('Ctrl Pts',(90.830767001692,1.69260502592648,0.542387424600279));
#5553=CARTESIAN_POINT('Ctrl Pts',(90.835061240625,1.67208360227967,0.602712333521105));
#5554=CARTESIAN_POINT('Ctrl Pts',(90.839355479558,1.64833651614558,0.661854056451308));
#5555=CARTESIAN_POINT('Ctrl Pts',(90.8437833128588,1.62385065487345,0.722835686571596));
#5556=CARTESIAN_POINT('Ctrl Pts',(90.8482111461596,1.59593513686523,0.782558742003975));
#5557=CARTESIAN_POINT('Ctrl Pts',(90.8526389794605,1.56474685617675,0.840613667855199));
#5558=CARTESIAN_POINT('Ctrl Pts',(90.8569212506853,1.53458386948086,0.896760076615978));
#5559=CARTESIAN_POINT('Ctrl Pts',(90.8612035219102,1.50136022647957,0.951345849076749));
#5560=CARTESIAN_POINT('Ctrl Pts',(90.865485793135,1.46526665824609,1.00402075811825));
#5561=CARTESIAN_POINT('Ctrl Pts',(90.8697654007131,1.42919554083589,1.05666290245588));
#5562=CARTESIAN_POINT('Ctrl Pts',(90.8740450082913,1.39025832290734,1.1073961244502));
#5563=CARTESIAN_POINT('Ctrl Pts',(90.8783246158694,1.34869001932574,1.15589761409527));
#5564=CARTESIAN_POINT('Ctrl Pts',(90.8826031111121,1.30713251998172,1.20438649746172));
#5565=CARTESIAN_POINT('Ctrl Pts',(90.8868816063548,1.26294562097733,1.25064441647907));
#5566=CARTESIAN_POINT('Ctrl Pts',(90.8911601015975,1.21640447789817,1.29438178627841));
#5567=CARTESIAN_POINT('Ctrl Pts',(90.8954390339994,1.16985857943503,1.33812362498362));
#5568=CARTESIAN_POINT('Ctrl Pts',(90.8997179664013,1.12095832981624,1.37934405987335));
#5569=CARTESIAN_POINT('Ctrl Pts',(90.9039968988031,1.07001410762691,1.41779190009655));
#5570=CARTESIAN_POINT('Ctrl Pts',(90.9082805777271,1.01901337417435,1.45628238963161));
#5571=CARTESIAN_POINT('Ctrl Pts',(90.912564256651,0.965964549780858,1.4919938455216));
#5572=CARTESIAN_POINT('Ctrl Pts',(90.916847935575,0.911208309015228,1.52471750828854));
#5573=CARTESIAN_POINT('Ctrl Pts',(90.9211344824345,0.856415408785725,1.55746307964373));
#5574=CARTESIAN_POINT('Ctrl Pts',(90.9254210292941,0.799913265220529,1.58721664419762));
#5575=CARTESIAN_POINT('Ctrl Pts',(90.9297075761536,0.742065909822544,1.61381605146908));
#5576=CARTESIAN_POINT('Ctrl Pts',(90.9340013842004,0.684120564016517,1.64046051675147));
#5577=CARTESIAN_POINT('Ctrl Pts',(90.9382951922471,0.62482593063744,1.6639399843529));
#5578=CARTESIAN_POINT('Ctrl Pts',(90.9425890002939,0.564563525786503,1.68414135031817));
#5579=CARTESIAN_POINT('Ctrl Pts',(90.943600493122,0.550367504528681,1.68890018829335));
#5580=CARTESIAN_POINT('Ctrl Pts',(90.94461198595,0.536117828318496,1.69347733604087));
#5581=CARTESIAN_POINT('Ctrl Pts',(90.9456234787781,0.52181956461287,1.69787172792506));
#5582=CARTESIAN_POINT('Ctrl Pts',(90.9508792364086,0.447525208302705,1.72070516582578));
#5583=CARTESIAN_POINT('Ctrl Pts',(90.956134994039,0.371672095356916,1.73867619936979));
#5584=CARTESIAN_POINT('Ctrl Pts',(90.9613907516695,0.294836286418164,1.75160943897638));
#5585=CARTESIAN_POINT('Ctrl Pts',(90.9665711570939,0.219102078450892,1.76435725372037));
#5586=CARTESIAN_POINT('Ctrl Pts',(90.9717515625183,0.1424131311743,1.77221064472054));
#5587=CARTESIAN_POINT('Ctrl Pts',(90.9769319679427,0.0653420109390083,1.77504774135978));
#5588=CARTESIAN_POINT('Ctrl Pts',(90.9783601202927,0.0440947740017713,1.77582988211917));
#5589=CARTESIAN_POINT('Ctrl Pts',(90.9797882726427,0.0228186163093154,1.77623105384898));
#5590=CARTESIAN_POINT('Ctrl Pts',(90.9812164249928,0.00152582238372707,
1.77624934464901));
#5591=CARTESIAN_POINT('Ctrl Pts',(90.9812164250559,0.00152582144218705,
1.77624934464982));
#5592=CARTESIAN_POINT('Ctrl Pts',(90.9854749319705,-0.0619656612165415,
1.77630388466468));
#5593=CARTESIAN_POINT('Ctrl Pts',(90.9897334388851,-0.125518642809964,1.77294990638981));
#5594=CARTESIAN_POINT('Ctrl Pts',(90.9939919457997,-0.188737306903355,1.76619429607359));
#5595=CARTESIAN_POINT('Ctrl Pts',(90.9982487764536,-0.251931086463013,1.75944134494378));
#5596=CARTESIAN_POINT('Ctrl Pts',(91.0025056071076,-0.314790302202684,1.74928947146205));
#5597=CARTESIAN_POINT('Ctrl Pts',(91.0067624377615,-0.376923173624967,1.73579750653251));
#5598=CARTESIAN_POINT('Ctrl Pts',(91.0110191723997,-0.439054643597801,1.72230584592348));
#5599=CARTESIAN_POINT('Ctrl Pts',(91.0152759070379,-0.500459303301463,1.70547435420072));
#5600=CARTESIAN_POINT('Ctrl Pts',(91.0195326416762,-0.560756541552351,1.6854127576372));
#5601=CARTESIAN_POINT('Ctrl Pts',(91.023793808635,-0.621116564241113,1.66533027195671));
#5602=CARTESIAN_POINT('Ctrl Pts',(91.0280549755938,-0.680366378618047,1.64201113055681));
#5603=CARTESIAN_POINT('Ctrl Pts',(91.0323161425526,-0.738142707939781,1.61561425012759));
#5604=CARTESIAN_POINT('Ctrl Pts',(91.036579751792,-0.795952151666422,1.58920224037123));
#5605=CARTESIAN_POINT('Ctrl Pts',(91.0408433610314,-0.852285977784346,1.55970921940593));
#5606=CARTESIAN_POINT('Ctrl Pts',(91.0451069702709,-0.906805755943714,1.5273399698454));
#5607=CARTESIAN_POINT('Ctrl Pts',(91.0493782819981,-0.961424027633953,1.49491224312689));
#5608=CARTESIAN_POINT('Ctrl Pts',(91.0536495937254,-1.01422128714294,1.45959820236663));
#5609=CARTESIAN_POINT('Ctrl Pts',(91.0579209054526,-1.06488920516866,1.42164518893262));
#5610=CARTESIAN_POINT('Ctrl Pts',(91.0602053352342,-1.0919879767638,1.40134674205597));
#5611=CARTESIAN_POINT('Ctrl Pts',(91.0624897650158,-1.11847824373169,1.38029410984162));
#5612=CARTESIAN_POINT('Ctrl Pts',(91.0647741947973,-1.14431715305377,1.35852946811135));
#5613=CARTESIAN_POINT('Ctrl Pts',(91.0690737655509,-1.19294907850031,1.31756580277999));
#5614=CARTESIAN_POINT('Ctrl Pts',(91.0733733363045,-1.23947723262404,1.27390443676415));
#5615=CARTESIAN_POINT('Ctrl Pts',(91.0776729070581,-1.28358730356138,1.22778976076363));
#5616=CARTESIAN_POINT('Ctrl Pts',(91.0821000738813,-1.3290064055644,1.18030656410139));
#5617=CARTESIAN_POINT('Ctrl Pts',(91.0865272407046,-1.37186114746335,1.13022239935008));
#5618=CARTESIAN_POINT('Ctrl Pts',(91.0909544075278,-1.41184454676913,1.07784926509149));
#5619=CARTESIAN_POINT('Ctrl Pts',(91.0952422023726,-1.45056922561345,1.02712489349108));
#5620=CARTESIAN_POINT('Ctrl Pts',(91.0995299972175,-1.48660034009003,0.974253971554576));
#5621=CARTESIAN_POINT('Ctrl Pts',(91.1038177920623,-1.51969766000126,0.919555917107115));
#5622=CARTESIAN_POINT('Ctrl Pts',(91.1081029792507,-1.55277485151513,0.864891127714878));
#5623=CARTESIAN_POINT('Ctrl Pts',(91.112388166439,-1.58292152656567,0.808401839493629));
#5624=CARTESIAN_POINT('Ctrl Pts',(91.1166733536274,-1.60994076449013,0.750436404589313));
#5625=CARTESIAN_POINT('Ctrl Pts',(91.1209574757118,-1.63695328665184,0.692485377275248));
#5626=CARTESIAN_POINT('Ctrl Pts',(91.1252415977961,-1.66083970214394,0.633059387996253));
#5627=CARTESIAN_POINT('Ctrl Pts',(91.1295257198804,-1.68144995841518,0.572529562420654));
#5628=CARTESIAN_POINT('Ctrl Pts',(91.1338103176526,-1.70206250314828,0.511993015909827));
#5629=CARTESIAN_POINT('Ctrl Pts',(91.1380949154249,-1.71939800743963,0.450352867635421));
#5630=CARTESIAN_POINT('Ctrl Pts',(91.1423795131971,-1.73335594783436,0.387996418291795));
#5631=CARTESIAN_POINT('Ctrl Pts',(91.1466688784554,-1.74732941927524,0.325570584722028));
#5632=CARTESIAN_POINT('Ctrl Pts',(91.1509582437136,-1.75791772080779,0.262427352657418));
#5633=CARTESIAN_POINT('Ctrl Pts',(91.1552476089719,-1.76507149025372,0.198964059049623));
#5634=CARTESIAN_POINT('Ctrl Pts',(91.1595398611743,-1.77223007452218,0.135458051667291));
#5635=CARTESIAN_POINT('Ctrl Pts',(91.1638321133766,-1.77594949939217,0.0716320567027389));
#5636=CARTESIAN_POINT('Ctrl Pts',(91.168124365579,-1.77623249677777,0.00788542266422285));
#5637=CARTESIAN_POINT('Ctrl Pts',(91.1724238554985,-1.77651597136158,-0.0559687027535952));
#5638=CARTESIAN_POINT('Ctrl Pts',(91.1767233454181,-1.77335148746199,-0.119742698575047));
#5639=CARTESIAN_POINT('Ctrl Pts',(91.1810228353376,-1.76679366480799,-0.183041548546642));
#5640=CARTESIAN_POINT('Ctrl Pts',(91.1819901938306,-1.76531819549464,-0.197283396127977));
#5641=CARTESIAN_POINT('Ctrl Pts',(91.1829575523235,-1.7636711524572,-0.211501233370493));
#5642=CARTESIAN_POINT('Ctrl Pts',(91.1839249108164,-1.76185351127122,-0.225690645178881));
#5643=CARTESIAN_POINT('Ctrl Pts',(91.1882231241585,-1.75377728135864,-0.288737715729961));
#5644=CARTESIAN_POINT('Ctrl Pts',(91.1925213375006,-1.74229612461739,-0.351479443022377));
#5645=CARTESIAN_POINT('Ctrl Pts',(91.1968195508426,-1.72744485579698,-0.413519446556672));
#5646=CARTESIAN_POINT('Ctrl Pts',(91.2012468873423,-1.71214743817654,-0.477423201496006));
#5647=CARTESIAN_POINT('Ctrl Pts',(91.2056742238421,-1.69327413474614,-0.540581848403752));
#5648=CARTESIAN_POINT('Ctrl Pts',(91.2101015603418,-1.67092064643609,-0.60256805077403));
#5649=CARTESIAN_POINT('Ctrl Pts',(91.2143879366153,-1.64927886205207,-0.662580698816891));
#5650=CARTESIAN_POINT('Ctrl Pts',(91.2186743128888,-1.62437536707959,-0.72149392708246));
#5651=CARTESIAN_POINT('Ctrl Pts',(91.2229606891622,-1.59634820683966,-0.778932901487549));
#5652=CARTESIAN_POINT('Ctrl Pts',(91.2272444390262,-1.56833821980045,-0.836336681066321));
#5653=CARTESIAN_POINT('Ctrl Pts',(91.2315281888903,-1.53720858364255,-0.892267546083985));
#5654=CARTESIAN_POINT('Ctrl Pts',(91.2358119387542,-1.50314513970486,-0.946371360239546));
#5655=CARTESIAN_POINT('Ctrl Pts',(91.2400946070401,-1.46909029624063,-1.00046151404948));
#5656=CARTESIAN_POINT('Ctrl Pts',(91.2443772753259,-1.43210338390166,-1.05272510635283));
#5657=CARTESIAN_POINT('Ctrl Pts',(91.2486599436117,-1.3924147911509,-1.10283503384875));
#5658=CARTESIAN_POINT('Ctrl Pts',(91.2529430733713,-1.35272192180399,-1.15295036087911));
#5659=CARTESIAN_POINT('Ctrl Pts',(91.2572262031309,-1.31032710974795,-1.20091116947056));
#5660=CARTESIAN_POINT('Ctrl Pts',(91.2615093328904,-1.26550118595883,-1.24642320695532));
#5661=CARTESIAN_POINT('Ctrl Pts',(91.2657972184817,-1.22062548909183,-1.2919857793537));
#5662=CARTESIAN_POINT('Ctrl Pts',(91.270085104073,-1.1733136507143,-1.33509379785901));
#5663=CARTESIAN_POINT('Ctrl Pts',(91.2743729896643,-1.12387266717102,-1.37549056357574));
#5664=CARTESIAN_POINT('Ctrl Pts',(91.2786637536486,-1.07439849464054,-1.41591444703253));
#5665=CARTESIAN_POINT('Ctrl Pts',(91.2829545176329,-1.02279274071359,-1.4536231603876));
#5666=CARTESIAN_POINT('Ctrl Pts',(91.2872452816171,-0.969392325396927,-1.48840269482474));
#5667=CARTESIAN_POINT('Ctrl Pts',(91.29154328421,-0.915901822462332,-1.52324090306416));
#5668=CARTESIAN_POINT('Ctrl Pts',(91.2958412868029,-0.860611055822227,-1.55513982642731));
#5669=CARTESIAN_POINT('Ctrl Pts',(91.3001392893958,-0.803881423270245,-1.58393141259999));
#5670=CARTESIAN_POINT('Ctrl Pts',(91.3011180685424,-0.790962449831687,-1.59048808713297));
#5671=CARTESIAN_POINT('Ctrl Pts',(91.302096847689,-0.777968932998481,-1.59688381334398));
#5672=CARTESIAN_POINT('Ctrl Pts',(91.3030756268356,-0.764905266538352,-1.60311696258317));
#5673=CARTESIAN_POINT('Ctrl Pts',(91.3073745691009,-0.707527718110618,-1.63049387268879));
#5674=CARTESIAN_POINT('Ctrl Pts',(91.3116735113661,-0.648561767975585,-1.65484218375743));
#5675=CARTESIAN_POINT('Ctrl Pts',(91.3159724536313,-0.588359603674145,-1.67597644352909));
#5676=CARTESIAN_POINT('Ctrl Pts',(91.3203996990156,-0.526360689154039,-1.69774146111995));
#5677=CARTESIAN_POINT('Ctrl Pts',(91.3248269443999,-0.463051030788027,-1.71609718988282));
#5678=CARTESIAN_POINT('Ctrl Pts',(91.3292541897843,-0.398841581838443,-1.73089267578802));
#5679=CARTESIAN_POINT('Ctrl Pts',(91.3335413175578,-0.336664293701429,-1.74521990029008));
#5680=CARTESIAN_POINT('Ctrl Pts',(91.3378284453313,-0.273643854694677,-1.75620876014265));
#5681=CARTESIAN_POINT('Ctrl Pts',(91.3421155731048,-0.210170241194075,-1.76377224499549));
#5682=CARTESIAN_POINT('Ctrl Pts',(91.3464000807608,-0.146735420174489,-1.77133110735519));
#5683=CARTESIAN_POINT('Ctrl Pts',(91.3506845884169,-0.0828484731931914,
-1.77546868675301));
#5684=CARTESIAN_POINT('Ctrl Pts',(91.3549690960729,-0.0189078653409894,
-1.77614936171715));
#5685=CARTESIAN_POINT('Ctrl Pts',(91.3592525272335,0.0450166772412661,-1.77682986565966));
#5686=CARTESIAN_POINT('Ctrl Pts',(91.3635359583942,0.10899435030359,-1.77405518402828));
#5687=CARTESIAN_POINT('Ctrl Pts',(91.3678193895548,0.172625282557775,-1.76784178430137));
#5688=CARTESIAN_POINT('Ctrl Pts',(91.3721032860686,0.236263127695454,-1.76162770954886));
#5689=CARTESIAN_POINT('Ctrl Pts',(91.3763871825825,0.299553656171313,-1.75197422745588));
#5690=CARTESIAN_POINT('Ctrl Pts',(91.3806710790963,0.36210270141522,-1.73894959562599));
#5691=CARTESIAN_POINT('Ctrl Pts',(91.3849597322688,0.424721198489555,-1.72591050179244));
#5692=CARTESIAN_POINT('Ctrl Pts',(91.3892483854413,0.486596076204566,-1.70949289526432));
#5693=CARTESIAN_POINT('Ctrl Pts',(91.3935370386137,0.547345140759118,-1.68981577676011));
#5694=CARTESIAN_POINT('Ctrl Pts',(91.3978285715565,0.608134997456195,-1.67012544534755));
#5695=CARTESIAN_POINT('Ctrl Pts',(91.4021201044993,0.667797067397921,-1.64717142917015));
#5696=CARTESIAN_POINT('Ctrl Pts',(91.406411637442,0.72596882539495,-1.62112100938045));
#5697=CARTESIAN_POINT('Ctrl Pts',(91.4107104040958,0.784238636393311,-1.59502667959156));
#5698=CARTESIAN_POINT('Ctrl Pts',(91.4150091707495,0.841012678882903,-1.56582576762878));
#5699=CARTESIAN_POINT('Ctrl Pts',(91.4193079374033,0.895953791088256,-1.533731028158));
#5700=CARTESIAN_POINT('Ctrl Pts',(91.4202807392204,0.908386848775099,-1.52646805638209));
#5701=CARTESIAN_POINT('Ctrl Pts',(91.4212535410375,0.920726165329498,-1.51905706017416));
#5702=CARTESIAN_POINT('Ctrl Pts',(91.4222263428547,0.932968059999427,-1.5115007977242));
#5703=CARTESIAN_POINT('Ctrl Pts',(91.4265252513526,0.987066216582616,-1.47810891842586));
#5704=CARTESIAN_POINT('Ctrl Pts',(91.4308241598505,1.03947950536856,-1.44174107480054));
#5705=CARTESIAN_POINT('Ctrl Pts',(91.4351230683485,1.08986123451802,-1.40259279621523));
#5706=CARTESIAN_POINT('Ctrl Pts',(91.4395144403953,1.14132660466173,-1.36260249254969));
#5707=CARTESIAN_POINT('Ctrl Pts',(91.4439058124422,1.19067150034813,-1.31971094349971));
#5708=CARTESIAN_POINT('Ctrl Pts',(91.4482971844891,1.23755467153794,-1.27417522243003));
#5709=CARTESIAN_POINT('Ctrl Pts',(91.4525842797451,1.28332456273594,-1.22972078502554));
#5710=CARTESIAN_POINT('Ctrl Pts',(91.4568713750012,1.32674796788167,-1.18274673913133));
#5711=CARTESIAN_POINT('Ctrl Pts',(91.4611584702572,1.3675401660274,-1.13353339465662));
#5712=CARTESIAN_POINT('Ctrl Pts',(91.4654429248555,1.40830723801461,-1.08435036338763));
#5713=CARTESIAN_POINT('Ctrl Pts',(91.4697273794537,1.44644599623708,-1.03293115604103));
#5714=CARTESIAN_POINT('Ctrl Pts',(91.474011834052,1.4817102738338,-0.979591101896785));
#5715=CARTESIAN_POINT('Ctrl Pts',(91.4782951917256,1.5169655229177,-0.926264704103836));
#5716=CARTESIAN_POINT('Ctrl Pts',(91.4825785493993,1.54934747463787,-0.871018855963951));
#5717=CARTESIAN_POINT('Ctrl Pts',(91.486861907073,1.57865294795679,-0.814198337266384));
#5718=CARTESIAN_POINT('Ctrl Pts',(91.4913330812731,1.6092434067058,-0.754886354334056));
#5719=CARTESIAN_POINT('Ctrl Pts',(91.4958042554731,1.63648104049615,-0.693858919280336));
#5720=CARTESIAN_POINT('Ctrl Pts',(91.5002754296732,1.66018901052115,-0.631535044035412));
#5721=CARTESIAN_POINT('Ctrl Pts',(91.5045639800986,1.68292863559235,-0.571756768857921));
#5722=CARTESIAN_POINT('Ctrl Pts',(91.508852530524,1.70242124843261,-0.510786427960019));
#5723=CARTESIAN_POINT('Ctrl Pts',(91.5131410809495,1.71856159337882,-0.449010147171809));
#5724=CARTESIAN_POINT('Ctrl Pts',(91.5174325578708,1.73471295245526,-0.387191710407141));
#5725=CARTESIAN_POINT('Ctrl Pts',(91.5217240347921,1.74750739301217,-0.324566733028707));
#5726=CARTESIAN_POINT('Ctrl Pts',(91.5260155117134,1.75689093212616,-0.261530715429101));
#5727=CARTESIAN_POINT('Ctrl Pts',(91.5303139690037,1.76628973418252,-0.198392165608831));
#5728=CARTESIAN_POINT('Ctrl Pts',(91.5346124262939,1.7722665268007,-0.134841742660515));
#5729=CARTESIAN_POINT('Ctrl Pts',(91.5389108835842,1.7748192920435,-0.0712779284927003));
#5730=CARTESIAN_POINT('Ctrl Pts',(91.5394459215473,1.77513704006881,-0.0633660076883157));
#5731=CARTESIAN_POINT('Ctrl Pts',(91.5399809595105,1.77540180472763,-0.0554538750348641));
#5732=CARTESIAN_POINT('Ctrl Pts',(91.5405159974736,1.77561363837197,-0.0475422940912406));
#5733=CARTESIAN_POINT('Origin',(88.3562164250559,0.,0.));
#5734=CARTESIAN_POINT('',(92.4383302476831,1.77320199105526,-0.0474633882366059));
#5735=CARTESIAN_POINT('',(92.2906253551795,1.77468168403539,-0.0475286896032536));
#5736=CARTESIAN_POINT('',(88.3562164250559,1.77561363837197,-0.0475422940912398));
#5737=CARTESIAN_POINT('',(91.8790868291566,-0.000950402920720204,1.77856749323898));
#5738=CARTESIAN_POINT('Ctrl Pts',(91.8790868291566,-0.000950402920720204,
1.77856749323898));
#5739=CARTESIAN_POINT('Ctrl Pts',(91.8827809065456,-0.0557221683725779,
1.7789218457455));
#5740=CARTESIAN_POINT('Ctrl Pts',(91.9261918892744,-0.699017003225842,1.75176962424819));
#5741=CARTESIAN_POINT('Ctrl Pts',(92.0093197773428,-1.8628457362405,0.969248007846431));
#5742=CARTESIAN_POINT('Ctrl Pts',(92.1284704933619,-1.82397533873842,-1.04055267810004));
#5743=CARTESIAN_POINT('Ctrl Pts',(92.2476212093811,-0.113688812436545,-2.09683346434928));
#5744=CARTESIAN_POINT('Ctrl Pts',(92.3509077941549,1.45919325958565,-1.34685406637966));
#5745=CARTESIAN_POINT('Ctrl Pts',(92.4144774735888,1.76180986717413,-0.403366942278606));
#5746=CARTESIAN_POINT('Ctrl Pts',(92.4383302476831,1.77320199105525,-0.0474633882366439));
#5747=CARTESIAN_POINT('Ctrl Pts',(91.8777557556434,-0.00103318020657592,
1.77624969951825));
#5748=CARTESIAN_POINT('Ctrl Pts',(91.8707368718479,0.109507008580014,1.77631399674803));
#5749=CARTESIAN_POINT('Ctrl Pts',(91.8640538279637,0.219824095479598,1.76605951654221));
#5750=CARTESIAN_POINT('Ctrl Pts',(91.8519898096994,0.412189196020058,1.72986097897984));
#5751=CARTESIAN_POINT('Ctrl Pts',(91.846680475189,0.494645281326305,1.70811082915314));
#5752=CARTESIAN_POINT('Ctrl Pts',(91.83951860179,0.599650062392536,1.67216947119991));
#5753=CARTESIAN_POINT('Ctrl Pts',(91.8378365911201,0.623896042496529,1.66327524938476));
#5754=CARTESIAN_POINT('Ctrl Pts',(91.8351863225811,0.661390960938906,1.64858569769984));
#5755=CARTESIAN_POINT('Ctrl Pts',(91.8342301316928,0.674778216568841,1.64315158873551));
#5756=CARTESIAN_POINT('Ctrl Pts',(91.832435126572,0.699637814510184,1.63270563433127));
#5757=CARTESIAN_POINT('Ctrl Pts',(91.8315977433032,0.711126414284918,1.62773461255972));
#5758=CARTESIAN_POINT('Ctrl Pts',(91.8297118721351,0.736751081864573,1.61632397214454));
#5759=CARTESIAN_POINT('Ctrl Pts',(91.8286612102891,0.750856995888474,1.60981958135189));
#5760=CARTESIAN_POINT('Ctrl Pts',(91.8259434306869,0.786899469107592,1.59262323375946));
#5761=CARTESIAN_POINT('Ctrl Pts',(91.8242671835355,0.808703643108505,1.58166300264375));
#5762=CARTESIAN_POINT('Ctrl Pts',(91.8145418753254,0.93273275792427,1.51608256608761));
#5763=CARTESIAN_POINT('Ctrl Pts',(91.8061626329232,1.0296263861501,1.45201853769499));
#5764=CARTESIAN_POINT('Ctrl Pts',(91.7921925889266,1.17798832582408,1.331566174817));
#5765=CARTESIAN_POINT('Ctrl Pts',(91.7866751450469,1.23333018416285,1.28047747329819));
#5766=CARTESIAN_POINT('Ctrl Pts',(91.7794304657962,1.30308532221069,1.2073521040174));
#5767=CARTESIAN_POINT('Ctrl Pts',(91.7775956144617,1.32049517270121,1.18828578136537));
#5768=CARTESIAN_POINT('Ctrl Pts',(91.7744717417336,1.34977891659175,1.15477704813706));
#5769=CARTESIAN_POINT('Ctrl Pts',(91.7731721720948,1.36185163924426,1.1405145051594));
#5770=CARTESIAN_POINT('Ctrl Pts',(91.7712740418605,1.37935182975643,1.11916582287923));
#5771=CARTESIAN_POINT('Ctrl Pts',(91.7706641470608,1.38495414045629,1.11222553773524));
#5772=CARTESIAN_POINT('Ctrl Pts',(91.7695783802573,1.3948944191896,1.09971969407853));
#5773=CARTESIAN_POINT('Ctrl Pts',(91.7691011916088,1.39925175680091,1.0941701750966));
#5774=CARTESIAN_POINT('Ctrl Pts',(91.7680341564229,1.40896918169565,1.08164104164261));
#5775=CARTESIAN_POINT('Ctrl Pts',(91.7674455935812,1.41431059633009,1.07464740415189));
#5776=CARTESIAN_POINT('Ctrl Pts',(91.7656596544044,1.43045248538915,1.05318363424268));
#5777=CARTESIAN_POINT('Ctrl Pts',(91.764473134501,1.44108486569628,1.03858776808788));
#5778=CARTESIAN_POINT('Ctrl Pts',(91.7577880790405,1.50031744818914,0.954613317933439));
#5779=CARTESIAN_POINT('Ctrl Pts',(91.752543651256,1.54413376610337,0.881982610982947));
#5780=CARTESIAN_POINT('Ctrl Pts',(91.7426013691406,1.61753349565499,0.737948589834908));
#5781=CARTESIAN_POINT('Ctrl Pts',(91.7379076574362,1.64797336191563,0.667207743810491));
#5782=CARTESIAN_POINT('Ctrl Pts',(91.7288392094935,1.69675312593909,0.529925381656571));
#5783=CARTESIAN_POINT('Ctrl Pts',(91.7244918029674,1.71599135168586,0.463857919493194));
#5784=CARTESIAN_POINT('Ctrl Pts',(91.7186962456932,1.73590228256272,0.376991095390475));
#5785=CARTESIAN_POINT('Ctrl Pts',(91.7173613993357,1.74011136719097,0.357059370934363));
#5786=CARTESIAN_POINT('Ctrl Pts',(91.7151362191763,1.74650257608371,0.323990753469435));
#5787=CARTESIAN_POINT('Ctrl Pts',(91.7142522013224,1.74888148861618,0.310893517115));
#5788=CARTESIAN_POINT('Ctrl Pts',(91.7125152829974,1.75324258674415,0.285247052917134));
#5789=CARTESIAN_POINT('Ctrl Pts',(91.7116628538573,1.75523778736061,0.272700833232157));
#5790=CARTESIAN_POINT('Ctrl Pts',(91.7095997191405,1.75971793371518,0.242439353121466));
#5791=CARTESIAN_POINT('Ctrl Pts',(91.7083848997398,1.76207013059135,0.224706163995916));
#5792=CARTESIAN_POINT('Ctrl Pts',(91.7042214800063,1.76916288372251,0.164241067954009));
#5793=CARTESIAN_POINT('Ctrl Pts',(91.7012335637153,1.77261940804443,0.121376792252211));
#5794=CARTESIAN_POINT('Ctrl Pts',(91.6952385851482,1.77637357342182,0.0364394768755772));
#5795=CARTESIAN_POINT('Ctrl Pts',(91.6922370670237,1.77673722724866,-0.00557874564042932));
#5796=CARTESIAN_POINT('Ctrl Pts',(91.6892085678292,1.77561362793331,-0.0475426839535299));
#5797=CARTESIAN_POINT('',(91.7312164509562,-0.000866965636682646,1.77616513543833));
#5798=CARTESIAN_POINT('Ctrl Pts',(91.5405159974736,1.77561363837197,-0.0475422940912406));
#5799=CARTESIAN_POINT('Ctrl Pts',(91.5408030179403,1.77572727627368,-0.0432981360846548));
#5800=CARTESIAN_POINT('Ctrl Pts',(91.5410900384071,1.77582568204212,-0.0390541368196787));
#5801=CARTESIAN_POINT('Ctrl Pts',(91.5413770588738,1.77590886522354,-0.0348104139653638));
#5802=CARTESIAN_POINT('Ctrl Pts',(91.5456757924709,1.77715470786581,0.0287482382035046));
#5803=CARTESIAN_POINT('Ctrl Pts',(91.549974526068,1.77498669166783,0.0925033035107822));
#5804=CARTESIAN_POINT('Ctrl Pts',(91.5542732596652,1.76938128301735,0.156057482383559));
#5805=CARTESIAN_POINT('Ctrl Pts',(91.558700531133,1.76360826516845,0.221512016010193));
#5806=CARTESIAN_POINT('Ctrl Pts',(91.5631278026008,1.75418888579952,0.286752923207428));
#5807=CARTESIAN_POINT('Ctrl Pts',(91.5675550740686,1.74115529809571,0.351343550407898));
#5808=CARTESIAN_POINT('Ctrl Pts',(91.571841988888,1.72853491087002,0.413886477569995));
#5809=CARTESIAN_POINT('Ctrl Pts',(91.5761289037074,1.71252616655278,0.475819205086708));
#5810=CARTESIAN_POINT('Ctrl Pts',(91.5804158185268,1.69321079658883,0.536750650502649));
#5811=CARTESIAN_POINT('Ctrl Pts',(91.5847001122304,1.6739072364748,0.597644841067788));
#5812=CARTESIAN_POINT('Ctrl Pts',(91.588984405934,1.65130121199289,0.657538484231631));
#5813=CARTESIAN_POINT('Ctrl Pts',(91.5932686996377,1.62552476460653,0.716053979914141));
#5814=CARTESIAN_POINT('Ctrl Pts',(91.597551916192,1.59975479788712,0.774554763738437));
#5815=CARTESIAN_POINT('Ctrl Pts',(91.6018351327464,1.5708161936863,0.831677626948991));
#5816=CARTESIAN_POINT('Ctrl Pts',(91.6061183493008,1.53888901708276,0.887065192419401));
#5817=CARTESIAN_POINT('Ctrl Pts',(91.6104020308983,1.50695837403931,0.942458771502284));
#5818=CARTESIAN_POINT('Ctrl Pts',(91.6146857124958,1.47203876905022,0.996116244024471));
#5819=CARTESIAN_POINT('Ctrl Pts',(91.6189693940932,1.43435508267371,1.04770680980325));
#5820=CARTESIAN_POINT('Ctrl Pts',(91.6232578332735,1.39662954368612,1.09935467358263));
#5821=CARTESIAN_POINT('Ctrl Pts',(91.6275462724539,1.35613409809761,1.14893064454811));
#5822=CARTESIAN_POINT('Ctrl Pts',(91.6318347116342,1.31313490030285,1.19613577661845));
#5823=CARTESIAN_POINT('Ctrl Pts',(91.6361260308787,1.27010682476358,1.24337261108821));
#5824=CARTESIAN_POINT('Ctrl Pts',(91.6404173501233,1.22457201107376,1.28823508618731));
#5825=CARTESIAN_POINT('Ctrl Pts',(91.6447086693678,1.17683246650155,1.33046210328888));
#5826=CARTESIAN_POINT('Ctrl Pts',(91.6490072246725,1.12901242309016,1.37276032395742));
#5827=CARTESIAN_POINT('Ctrl Pts',(91.6533057799772,1.07898062884179,1.41241391212508));
#5828=CARTESIAN_POINT('Ctrl Pts',(91.657604335282,1.02707003592149,1.44920364470016));
#5829=CARTESIAN_POINT('Ctrl Pts',(91.6585788151523,1.01530193611311,1.45754385467487));
#5830=CARTESIAN_POINT('Ctrl Pts',(91.6595532950226,1.00343738422584,1.46573706813981));
#5831=CARTESIAN_POINT('Ctrl Pts',(91.660527774893,0.991480433293622,1.47378106002754));
#5832=CARTESIAN_POINT('Ctrl Pts',(91.6648979419894,0.937858111141657,1.50985526714243));
#5833=CARTESIAN_POINT('Ctrl Pts',(91.6692681090858,0.88216220231501,1.54306827283372));
#5834=CARTESIAN_POINT('Ctrl Pts',(91.6736382761822,0.824724424407,1.5731794831762));
#5835=CARTESIAN_POINT('Ctrl Pts',(91.6780010643716,0.767383628608955,1.60323985156729));
#5836=CARTESIAN_POINT('Ctrl Pts',(91.6823638525609,0.70830722561498,1.63020859975998));
#5837=CARTESIAN_POINT('Ctrl Pts',(91.6867266407503,0.647855562855665,1.65388851866653));
#5838=CARTESIAN_POINT('Ctrl Pts',(91.6910823738664,0.587501656597596,1.67753014473023));
#5839=CARTESIAN_POINT('Ctrl Pts',(91.6954381069825,0.525777357976388,1.69789333956063));
#5840=CARTESIAN_POINT('Ctrl Pts',(91.6997938400986,0.463065448793341,1.71482782011309));
#5841=CARTESIAN_POINT('Ctrl Pts',(91.704145446695,0.400412951406215,1.73174625733478));
#5842=CARTESIAN_POINT('Ctrl Pts',(91.7084970532914,0.336775164611691,1.74524230409755));
#5843=CARTESIAN_POINT('Ctrl Pts',(91.7128486598878,0.272551386052349,1.75521503083267));
#5844=CARTESIAN_POINT('Ctrl Pts',(91.7171974553322,0.208369096262898,1.76518131515388));
#5845=CARTESIAN_POINT('Ctrl Pts',(91.7215462507766,0.143602042190318,1.77162872716101));
#5846=CARTESIAN_POINT('Ctrl Pts',(91.725895046221,0.0786594231437778,1.77450746903209));
#5847=CARTESIAN_POINT('Ctrl Pts',(91.7276688391659,0.0521705342173203,1.77568165440975));
#5848=CARTESIAN_POINT('Ctrl Pts',(91.7294426321109,0.0256525205454586,1.77626272710031));
#5849=CARTESIAN_POINT('Ctrl Pts',(91.7312164250558,-0.000866620254329586,
1.77624978859093));
#5850=CARTESIAN_POINT('Ctrl Pts',(91.7312171833216,-0.000876731753600045,
1.77377146193875));
#5851=CARTESIAN_POINT('Ctrl Pts',(91.7473709525184,-0.242047698959972,1.77483106190353));
#5852=CARTESIAN_POINT('Ctrl Pts',(91.8032416270549,-1.07484492687079,1.61655950001718));
#5853=CARTESIAN_POINT('Ctrl Pts',(91.8988292069313,-2.07083606885155,0.348244089557057));
#5854=CARTESIAN_POINT('Ctrl Pts',(92.0179799229503,-1.41471804329461,-1.55184057332674));
#5855=CARTESIAN_POINT('Ctrl Pts',(92.1371306389695,0.537789440227507,-2.02988107712031));
#5856=CARTESIAN_POINT('Ctrl Pts',(92.2280124497125,1.65117025021109,-0.975720506046015));
#5857=CARTESIAN_POINT('Ctrl Pts',(92.2791773551159,1.77170285356651,-0.21804953119594));
#5858=CARTESIAN_POINT('Ctrl Pts',(92.2906253551795,1.77468168403539,-0.047528689603001));
#5859=CARTESIAN_POINT('Origin',(88.3562164250559,0.,0.));
#5860=CARTESIAN_POINT('',(93.1883366943682,1.77561363837197,-0.047542294091239));
#5861=CARTESIAN_POINT('',(93.0389806716277,1.77561363837854,-0.0475422938458683));
#5862=CARTESIAN_POINT('',(88.3562164250559,1.77561363837197,-0.0475422940912398));
#5863=CARTESIAN_POINT('',(92.6290868540185,0.00157867016090192,1.77624929846588));
#5864=CARTESIAN_POINT('Ctrl Pts',(92.6290868540186,0.00157867016090192,
1.77624929846588));
#5865=CARTESIAN_POINT('Ctrl Pts',(92.6333154763636,-0.0612556274311389,
1.77630514345947));
#5866=CARTESIAN_POINT('Ctrl Pts',(92.6375440987086,-0.124197499503331,1.7730226365899));
#5867=CARTESIAN_POINT('Ctrl Pts',(92.6417727210536,-0.186857609780307,1.76639415085286));
#5868=CARTESIAN_POINT('Ctrl Pts',(92.6459976525732,-0.249463029071135,1.75977145058954));
#5869=CARTESIAN_POINT('Ctrl Pts',(92.6502225840928,-0.311786659069597,1.74980860976227));
#5870=CARTESIAN_POINT('Ctrl Pts',(92.6544475156124,-0.373440848285772,1.73655002672874));
#5871=CARTESIAN_POINT('Ctrl Pts',(92.6586703829559,-0.435064915094421,1.72329792144549));
#5872=CARTESIAN_POINT('Ctrl Pts',(92.6628932502993,-0.496019681904808,1.70675337422147));
#5873=CARTESIAN_POINT('Ctrl Pts',(92.6671161176427,-0.555926481664665,1.68701209523938));
#5874=CARTESIAN_POINT('Ctrl Pts',(92.6713385441744,-0.615827027943092,1.66727287698698));
#5875=CARTESIAN_POINT('Ctrl Pts',(92.6755609707061,-0.674679331323129,1.64433775375019));
#5876=CARTESIAN_POINT('Ctrl Pts',(92.6797833972377,-0.732120831172046,1.61835198614639));
#5877=CARTESIAN_POINT('Ctrl Pts',(92.6840098160817,-0.78961664206863,1.59234164894975));
#5878=CARTESIAN_POINT('Ctrl Pts',(92.6882362349257,-0.84569851279654,1.5632751255513));
#5879=CARTESIAN_POINT('Ctrl Pts',(92.6924626537697,-0.900026111334196,1.53134485385123));
#5880=CARTESIAN_POINT('Ctrl Pts',(92.6966912893475,-0.954382204402451,1.49939783489694));
#5881=CARTESIAN_POINT('Ctrl Pts',(92.7009199249252,-1.00698176234783,1.46458436810422));
#5882=CARTESIAN_POINT('Ctrl Pts',(92.7051485605029,-1.05751387769493,1.42713995844228));
#5883=CARTESIAN_POINT('Ctrl Pts',(92.709384550352,-1.10813387644569,1.38963042698311));
#5884=CARTESIAN_POINT('Ctrl Pts',(92.7136205402011,-1.15667885988232,1.34948115599194));
#5885=CARTESIAN_POINT('Ctrl Pts',(92.7178565300502,-1.20287236373434,1.3069667704514));
#5886=CARTESIAN_POINT('Ctrl Pts',(92.7199790445193,-1.22601840133124,1.28566421740665));
#5887=CARTESIAN_POINT('Ctrl Pts',(92.7221015589885,-1.24857465810838,1.26376841918942));
#5888=CARTESIAN_POINT('Ctrl Pts',(92.7242240734576,-1.27051017199142,1.24131702854925));
#5889=CARTESIAN_POINT('Ctrl Pts',(92.7285228830294,-1.31493700554775,1.19584537010543));
#5890=CARTESIAN_POINT('Ctrl Pts',(92.7328216926012,-1.35701005379085,1.1478930620762));
#5891=CARTESIAN_POINT('Ctrl Pts',(92.737120502173,-1.39644013775725,1.0977335761288));
#5892=CARTESIAN_POINT('Ctrl Pts',(92.7415477641439,-1.43704842903952,1.04607527842757));
#5893=CARTESIAN_POINT('Ctrl Pts',(92.7459750261149,-1.47485283271129,0.992076099468365));
#5894=CARTESIAN_POINT('Ctrl Pts',(92.7504022880859,-1.50957782884443,0.936076300929225));
#5895=CARTESIAN_POINT('Ctrl Pts',(92.7546892817189,-1.54320263765496,0.881850736379493));
#5896=CARTESIAN_POINT('Ctrl Pts',(92.7589762753519,-1.5739399715431,0.82574989835249));
#5897=CARTESIAN_POINT('Ctrl Pts',(92.7632632689849,-1.60158163077267,0.76811479771682));
#5898=CARTESIAN_POINT('Ctrl Pts',(92.7675476423367,-1.62920639496417,0.710514924605348));
#5899=CARTESIAN_POINT('Ctrl Pts',(92.7718320156885,-1.65373901932468,0.651383101978016));
#5900=CARTESIAN_POINT('Ctrl Pts',(92.7761163890403,-1.67501720372595,0.591084959817191));
#5901=CARTESIAN_POINT('Ctrl Pts',(92.7803996859506,-1.69629004201977,0.53080196746149));
#5902=CARTESIAN_POINT('Ctrl Pts',(92.7846829828608,-1.71430989594296,0.469353712276196));
#5903=CARTESIAN_POINT('Ctrl Pts',(92.7889662797711,-1.72896331348721,0.407123965292314));
#5904=CARTESIAN_POINT('Ctrl Pts',(92.7932500423064,-1.74361832396242,0.344887453491231));
#5905=CARTESIAN_POINT('Ctrl Pts',(92.7975338048416,-1.75490605944284,0.28186977244651));
#5906=CARTESIAN_POINT('Ctrl Pts',(92.8018175673768,-1.76276392813596,0.21846600688138));
#5907=CARTESIAN_POINT('Ctrl Pts',(92.8061060878377,-1.7706305244734,0.154991819483508));
#5908=CARTESIAN_POINT('Ctrl Pts',(92.8103946082987,-1.77505959383456,0.0911311931016721));
#5909=CARTESIAN_POINT('Ctrl Pts',(92.8146831287597,-1.7760404364522,0.0272842552893976));
#5910=CARTESIAN_POINT('Ctrl Pts',(92.8189745295803,-1.77702193784703,-0.0366055649449436));
#5911=CARTESIAN_POINT('Ctrl Pts',(92.8232659304009,-1.77455062526379,-0.100481175186551));
#5912=CARTESIAN_POINT('Ctrl Pts',(92.8275573312215,-1.76866784348525,-0.163945484601535));
#5913=CARTESIAN_POINT('Ctrl Pts',(92.8318559678007,-1.76277514271052,-0.227516801596808));
#5914=CARTESIAN_POINT('Ctrl Pts',(92.8361546043798,-1.75345957497829,-0.290674937515888));
#5915=CARTESIAN_POINT('Ctrl Pts',(92.840453240959,-1.74081371049053,-0.353032134328007));
#5916=CARTESIAN_POINT('Ctrl Pts',(92.8414270904649,-1.73794880933956,-0.367159061363439));
#5917=CARTESIAN_POINT('Ctrl Pts',(92.8424009399708,-1.7349131854478,-0.381244943827301));
#5918=CARTESIAN_POINT('Ctrl Pts',(92.8433747894767,-1.73170826646264,-0.395285393563877));
#5919=CARTESIAN_POINT('Ctrl Pts',(92.8476735990735,-1.71756097121167,-0.45726336829579));
#5920=CARTESIAN_POINT('Ctrl Pts',(92.8519724086702,-1.70005337510742,-0.518607066947605));
#5921=CARTESIAN_POINT('Ctrl Pts',(92.8562712182669,-1.67925864640917,-0.578925263708581));
#5922=CARTESIAN_POINT('Ctrl Pts',(92.8606984802348,-1.6578425521565,-0.641045823477781));
#5923=CARTESIAN_POINT('Ctrl Pts',(92.8651257422027,-1.63293975690463,-0.702078069452736));
#5924=CARTESIAN_POINT('Ctrl Pts',(92.8695530041706,-1.60468696627331,-0.761606067972524));
#5925=CARTESIAN_POINT('Ctrl Pts',(92.8738399978295,-1.57732930477416,-0.819248049413498));
#5926=CARTESIAN_POINT('Ctrl Pts',(92.8781269914885,-1.54683099355722,-0.875479186541712));
#5927=CARTESIAN_POINT('Ctrl Pts',(92.8824139851475,-1.51336584339643,-0.929939721993324));
#5928=CARTESIAN_POINT('Ctrl Pts',(92.8866983585256,-1.47992114768489,-0.984366970271449));
#5929=CARTESIAN_POINT('Ctrl Pts',(92.8909827319036,-1.44351347241234,-1.0370253345937));
#5930=CARTESIAN_POINT('Ctrl Pts',(92.8952671052817,-1.40436218992483,-1.08758029681009));
#5931=CARTESIAN_POINT('Ctrl Pts',(92.8995504022186,-1.36522074412762,-1.13812255718188));
#5932=CARTESIAN_POINT('Ctrl Pts',(92.9038336991554,-1.3233373679364,-1.18656206631749));
#5933=CARTESIAN_POINT('Ctrl Pts',(92.9081169960923,-1.27897314805749,-1.23259553343663));
#5934=CARTESIAN_POINT('Ctrl Pts',(92.9124007586543,-1.23460410546924,-1.27863400472426));
#5935=CARTESIAN_POINT('Ctrl Pts',(92.9166845212163,-1.18775403591931,-1.32226555437649));
#5936=CARTESIAN_POINT('Ctrl Pts',(92.9209682837783,-1.1387210923156,-1.36322350933938));
#5937=CARTESIAN_POINT('Ctrl Pts',(92.9252568042662,-1.08963368838422,-1.40422695583273));
#5938=CARTESIAN_POINT('Ctrl Pts',(92.9295453247541,-1.03835896202669,-1.44255056134764));
#5939=CARTESIAN_POINT('Ctrl Pts',(92.933833845242,-0.985227420784922,-1.47796853546802));
#5940=CARTESIAN_POINT('Ctrl Pts',(92.9381252460897,-0.932060194053257,-1.51341029786423));
#5941=CARTESIAN_POINT('Ctrl Pts',(92.9424166469374,-0.877034105232559,-1.54594229080387));
#5942=CARTESIAN_POINT('Ctrl Pts',(92.9467080477851,-0.82050530832499,-1.57538411237086));
#5943=CARTESIAN_POINT('Ctrl Pts',(92.9510066843912,-0.763881197850672,-1.60487557598187));
#5944=CARTESIAN_POINT('Ctrl Pts',(92.9553053209974,-0.705749784086856,-1.6312662697093));
#5945=CARTESIAN_POINT('Ctrl Pts',(92.9596039576036,-0.646487131852348,-1.65442390300954));
#5946=CARTESIAN_POINT('Ctrl Pts',(92.960577806901,-0.63306127209009,-1.65967022806237));
#5947=CARTESIAN_POINT('Ctrl Pts',(92.9615516561985,-0.619577408992279,-1.66475082291976));
#5948=CARTESIAN_POINT('Ctrl Pts',(92.9625255054959,-0.60604000430414,-1.669664509919));
#5949=CARTESIAN_POINT('Ctrl Pts',(92.9668243150826,-0.546282580639698,-1.69135472916942));
#5950=CARTESIAN_POINT('Ctrl Pts',(92.9711231246693,-0.485237582363842,-1.70987697123046));
#5951=CARTESIAN_POINT('Ctrl Pts',(92.9754219342561,-0.423273476567525,-1.72508075942387));
#5952=CARTESIAN_POINT('Ctrl Pts',(92.9798491962252,-0.359457826325535,-1.74073885078556));
#5953=CARTESIAN_POINT('Ctrl Pts',(92.9842764581943,-0.294667731340171,-1.75287671939473));
#5954=CARTESIAN_POINT('Ctrl Pts',(92.9887037201634,-0.229326851357022,-1.76138390413523));
#5955=CARTESIAN_POINT('Ctrl Pts',(92.9929907138121,-0.166056157315864,-1.76962155693402));
#5956=CARTESIAN_POINT('Ctrl Pts',(92.9972777074609,-0.102269601256815,-1.77445508743876));
#5957=CARTESIAN_POINT('Ctrl Pts',(93.0015647011096,-0.0383637314043607,
-1.77583565867248));
#5958=CARTESIAN_POINT('Ctrl Pts',(93.0058490744773,0.0255030781299301,-1.77721538607837));
#5959=CARTESIAN_POINT('Ctrl Pts',(93.010133447845,0.0894885540990822,-1.77514632869863));
#5960=CARTESIAN_POINT('Ctrl Pts',(93.0144178212127,0.153192675496442,-1.76963161891797));
#5961=CARTESIAN_POINT('Ctrl Pts',(93.0187011181392,0.216880791345497,-1.76411829469843));
#5962=CARTESIAN_POINT('Ctrl Pts',(93.0229844150656,0.280287191138943,-1.75516108009091));
#5963=CARTESIAN_POINT('Ctrl Pts',(93.0272677119921,0.343015498596663,-1.74281508778828));
#5964=CARTESIAN_POINT('Ctrl Pts',(93.0315514745436,0.405750625071331,-1.73046775338774));
#5965=CARTESIAN_POINT('Ctrl Pts',(93.0358352370952,0.467807019197287,-1.71473101065585));
#5966=CARTESIAN_POINT('Ctrl Pts',(93.0401189996467,0.528798998452338,-1.69571096644912));
#5967=CARTESIAN_POINT('Ctrl Pts',(93.0444075201242,0.589858720799145,-1.67666979689746));
#5968=CARTESIAN_POINT('Ctrl Pts',(93.0486960406017,0.649851188524717,-1.65433820267206));
#5969=CARTESIAN_POINT('Ctrl Pts',(93.0529845610792,0.708407550322267,-1.62887163556445));
#5970=CARTESIAN_POINT('Ctrl Pts',(93.0572759619164,0.767003241158813,-1.60338796398552));
#5971=CARTESIAN_POINT('Ctrl Pts',(93.0615673627537,0.824160457267757,-1.57476535677365));
#5972=CARTESIAN_POINT('Ctrl Pts',(93.065858763591,0.879534600335056,-1.54320541384271));
#5973=CARTESIAN_POINT('Ctrl Pts',(93.0701574001868,0.935002110101268,-1.51159225748893));
#5974=CARTESIAN_POINT('Ctrl Pts',(93.0744560367826,0.988680128613843,-1.47703216068398));
#5975=CARTESIAN_POINT('Ctrl Pts',(93.0787546733784,1.04025370679951,-1.43976952599709));
#5976=CARTESIAN_POINT('Ctrl Pts',(93.0797285227573,1.05193762005059,-1.43132773455068));
#5977=CARTESIAN_POINT('Ctrl Pts',(93.0807023721362,1.06351366541221,-1.42274739559128));
#5978=CARTESIAN_POINT('Ctrl Pts',(93.0816762215151,1.07497843559964,-1.41403162110886));
#5979=CARTESIAN_POINT('Ctrl Pts',(93.086120407884,1.12729820546713,-1.37425696294458));
#5980=CARTESIAN_POINT('Ctrl Pts',(93.0905645942528,1.17751761796227,-1.33149086968185));
#5981=CARTESIAN_POINT('Ctrl Pts',(93.0950087806217,1.22527686049464,-1.2859862665038));
#5982=CARTESIAN_POINT('Ctrl Pts',(93.099299967917,1.27139190558409,-1.24204824077171));
#5983=CARTESIAN_POINT('Ctrl Pts',(93.1035911552123,1.31521299779926,-1.19555756077289));
#5984=CARTESIAN_POINT('Ctrl Pts',(93.1078823425076,1.35644716415272,-1.14678470227068));
#5985=CARTESIAN_POINT('Ctrl Pts',(93.112169235915,1.39764007039022,-1.09806064732084));
#5986=CARTESIAN_POINT('Ctrl Pts',(93.1164561293224,1.43625085980126,-1.04705932475888));
#5987=CARTESIAN_POINT('Ctrl Pts',(93.1207430227299,1.47202372930437,-0.994087623333509));
#5988=CARTESIAN_POINT('Ctrl Pts',(93.1250271698193,1.50777368158822,-0.941149857237133));
#5989=CARTESIAN_POINT('Ctrl Pts',(93.1293113169087,1.54068903955213,-0.886244633256476));
#5990=CARTESIAN_POINT('Ctrl Pts',(93.1335954639981,1.57055582273612,-0.82970987108125));
#5991=CARTESIAN_POINT('Ctrl Pts',(93.1378784086902,1.60041422344894,-0.773190976065579));
#5992=CARTESIAN_POINT('Ctrl Pts',(93.1421613533823,1.62722551427406,-0.715043896799184));
#5993=CARTESIAN_POINT('Ctrl Pts',(93.1464442980744,1.65082139094303,-0.655631602124937));
#5994=CARTESIAN_POINT('Ctrl Pts',(93.1507295910831,1.67443020511009,-0.596186731994426));
#5995=CARTESIAN_POINT('Ctrl Pts',(93.1550148840919,1.69481989690216,-0.535475729423321));
#5996=CARTESIAN_POINT('Ctrl Pts',(93.1593001771006,1.71187065899416,-0.473880691076261));
#5997=CARTESIAN_POINT('Ctrl Pts',(93.1635869163134,1.72892717539119,-0.412264865585633));
#5998=CARTESIAN_POINT('Ctrl Pts',(93.1678736555263,1.74264240457422,-0.349764901372216));
#5999=CARTESIAN_POINT('Ctrl Pts',(93.1721603947392,1.75294734932356,-0.286774568257931));
#6000=CARTESIAN_POINT('Ctrl Pts',(93.1764524215333,1.76326500495393,-0.223706538207797));
#6001=CARTESIAN_POINT('Ctrl Pts',(93.1807444483274,1.7701639253717,-0.160147432770856));
#6002=CARTESIAN_POINT('Ctrl Pts',(93.1850364751214,1.77362694173368,-0.0964962903765215));
#6003=CARTESIAN_POINT('Ctrl Pts',(93.1861365482037,1.77451453430148,-0.0801821078789996));
#6004=CARTESIAN_POINT('Ctrl Pts',(93.187236621286,1.77517667934864,-0.0638618768134948));
#6005=CARTESIAN_POINT('Ctrl Pts',(93.1883366943682,1.77561363837197,-0.0475422940912359));
#6006=CARTESIAN_POINT('Ctrl Pts',(92.4383302476831,1.77320199105525,-0.0474633882366439));
#6007=CARTESIAN_POINT('Ctrl Pts',(92.4541943789285,1.7807787260589,0.189242861096052));
#6008=CARTESIAN_POINT('Ctrl Pts',(92.5097754155136,1.6490061063227,1.02148169742008));
#6009=CARTESIAN_POINT('Ctrl Pts',(92.5733609426715,0.828714911293434,1.71278513326118));
#6010=CARTESIAN_POINT('Ctrl Pts',(92.621082338584,0.12056136551938,1.77794021860673));
#6011=CARTESIAN_POINT('Ctrl Pts',(92.6290868291567,0.00157956711881646,
1.77684271104738));
#6012=CARTESIAN_POINT('',(92.4812153597462,-0.0010931502662158,1.77831379137429));
#6013=CARTESIAN_POINT('Ctrl Pts',(92.2906253551795,1.77468168403539,-0.047528689603001));
#6014=CARTESIAN_POINT('Ctrl Pts',(92.3188942604556,1.7820374034528,0.373543767752086));
#6015=CARTESIAN_POINT('Ctrl Pts',(92.3824242619779,1.46982358280908,1.33346230864534));
#6016=CARTESIAN_POINT('Ctrl Pts',(92.4459542635001,0.521916176252472,1.77448723514747));
#6017=CARTESIAN_POINT('Ctrl Pts',(92.4812153597462,-0.0010931502662158,
1.77831379137429));
#6018=CARTESIAN_POINT('Ctrl Pts',(92.4824006868533,-0.00102231093804463,
1.77624970580725));
#6019=CARTESIAN_POINT('Ctrl Pts',(92.4845492905966,-0.0308338137244965,
1.77623254795761));
#6020=CARTESIAN_POINT('Ctrl Pts',(92.4866800846044,-0.0606420849328428,
1.77546488257387));
#6021=CARTESIAN_POINT('Ctrl Pts',(92.4900600408051,-0.108506512965212,1.77302521661446));
#6022=CARTESIAN_POINT('Ctrl Pts',(92.4913267374793,-0.126580022702816,1.77182663925871));
#6023=CARTESIAN_POINT('Ctrl Pts',(92.4931678342244,-0.153091812170338,1.76966069952318));
#6024=CARTESIAN_POINT('Ctrl Pts',(92.4937523798425,-0.161545936555108,1.76890898912668));
#6025=CARTESIAN_POINT('Ctrl Pts',(92.4947947242983,-0.176692663677203,1.7674526993751));
#6026=CARTESIAN_POINT('Ctrl Pts',(92.4952536823725,-0.183387201378406,1.76677063594963));
#6027=CARTESIAN_POINT('Ctrl Pts',(92.4961905783265,-0.197108315274421,1.76529384939534));
#6028=CARTESIAN_POINT('Ctrl Pts',(92.4966682223702,-0.204134026809555,1.76449521531135));
#6029=CARTESIAN_POINT('Ctrl Pts',(92.4977559852287,-0.220201914634042,1.76257147254318));
#6030=CARTESIAN_POINT('Ctrl Pts',(92.498364570249,-0.22924042489869,1.76141872240714));
#6031=CARTESIAN_POINT('Ctrl Pts',(92.5003155409023,-0.258356638486375,1.75747739097445));
#6032=CARTESIAN_POINT('Ctrl Pts',(92.501643747523,-0.278396401949765,1.75441456363633));
#6033=CARTESIAN_POINT('Ctrl Pts',(92.5074966346105,-0.367419455457645,1.73924460847041));
#6034=CARTESIAN_POINT('Ctrl Pts',(92.5118603367432,-0.43570968617708,1.7234059090987));
#6035=CARTESIAN_POINT('Ctrl Pts',(92.5199185636984,-0.561001786575576,1.68641988981419));
#6036=CARTESIAN_POINT('Ctrl Pts',(92.5236185218169,-0.618195851469421,1.66630400098528));
#6037=CARTESIAN_POINT('Ctrl Pts',(92.5326437004274,-0.753702442599686,1.61070544810568));
#6038=CARTESIAN_POINT('Ctrl Pts',(92.5379946540685,-0.830677246488275,1.57239063412253));
#6039=CARTESIAN_POINT('Ctrl Pts',(92.5452072081148,-0.926880391095909,1.51546315863747));
#6040=CARTESIAN_POINT('Ctrl Pts',(92.5468952372244,-0.948893826025128,1.50177769315874));
#6041=CARTESIAN_POINT('Ctrl Pts',(92.5495528525222,-0.982715258622012,1.47971080876184));
#6042=CARTESIAN_POINT('Ctrl Pts',(92.5505102582548,-0.994734096935685,1.47165804882015));
#6043=CARTESIAN_POINT('Ctrl Pts',(92.5523063093579,-1.016964628259,1.45636659146167));
#6044=CARTESIAN_POINT('Ctrl Pts',(92.5531435077076,-1.02720082871013,1.44916498284711));
#6045=CARTESIAN_POINT('Ctrl Pts',(92.5550273302939,-1.04994676311298,1.43280015880263));
#6046=CARTESIAN_POINT('Ctrl Pts',(92.5560761079423,-1.06241419502789,1.42358018811742));
#6047=CARTESIAN_POINT('Ctrl Pts',(92.5592547582628,-1.09960295474346,1.39531756746504));
#6048=CARTESIAN_POINT('Ctrl Pts',(92.561403622792,-1.12394361263514,1.37578643464634));
#6049=CARTESIAN_POINT('Ctrl Pts',(92.5731731089358,-1.2529044534201,1.26660024294768));
#6050=CARTESIAN_POINT('Ctrl Pts',(92.5832574740353,-1.34732281392176,1.16565625548978));
#6051=CARTESIAN_POINT('Ctrl Pts',(92.5987045445723,-1.47292661875574,0.995486829843145));
#6052=CARTESIAN_POINT('Ctrl Pts',(92.6040593281352,-1.51300256809924,0.933451742933734));
#6053=CARTESIAN_POINT('Ctrl Pts',(92.6104859292972,-1.55785274147325,0.853509464273474));
#6054=CARTESIAN_POINT('Ctrl Pts',(92.611727985458,-1.56636327041993,0.837788598602819));
#6055=CARTESIAN_POINT('Ctrl Pts',(92.6135588517891,-1.57869123875451,0.814171269895876));
#6056=CARTESIAN_POINT('Ctrl Pts',(92.614157916902,-1.58268959711021,0.80637121193379));
#6057=CARTESIAN_POINT('Ctrl Pts',(92.6151852269149,-1.58948753229712,0.792864328854585));
#6058=CARTESIAN_POINT('Ctrl Pts',(92.6156151172737,-1.59231439035989,0.78717173802353));
#6059=CARTESIAN_POINT('Ctrl Pts',(92.616621787836,-1.59889179991191,0.773746040087949));
#6060=CARTESIAN_POINT('Ctrl Pts',(92.6171970030907,-1.60261685703751,0.766000743864701));
#6061=CARTESIAN_POINT('Ctrl Pts',(92.6188658934207,-1.6133209839759,0.743324353929958));
#6062=CARTESIAN_POINT('Ctrl Pts',(92.61995088611,-1.62014885393761,0.728322340211201));
#6063=CARTESIAN_POINT('Ctrl Pts',(92.6285941527618,-1.67336603703679,0.606941641606831));
#6064=CARTESIAN_POINT('Ctrl Pts',(92.6356535983921,-1.70944311890215,0.496330273727835));
#6065=CARTESIAN_POINT('Ctrl Pts',(92.6487598942345,-1.75546517037981,0.287899998950804));
#6066=CARTESIAN_POINT('Ctrl Pts',(92.6547643035926,-1.76860351289484,0.191267654549485));
#6067=CARTESIAN_POINT('Ctrl Pts',(92.6630064392568,-1.77540991748136,0.0629020919228067));
#6068=CARTESIAN_POINT('Ctrl Pts',(92.6650282268388,-1.77624066832517,0.0317166686974413));
#6069=CARTESIAN_POINT('Ctrl Pts',(92.6680928712898,-1.77625452159584,-0.0149769166232618));
#6070=CARTESIAN_POINT('Ctrl Pts',(92.6691165253765,-1.77605613384216,-0.0304797886551062));
#6071=CARTESIAN_POINT('Ctrl Pts',(92.6709780469295,-1.77533088136162,-0.0584889915098783));
#6072=CARTESIAN_POINT('Ctrl Pts',(92.6718136462712,-1.7748747052451,-0.0709962487183724));
#6073=CARTESIAN_POINT('Ctrl Pts',(92.6736242825017,-1.77360626927814,-0.0979500158814898));
#6074=CARTESIAN_POINT('Ctrl Pts',(92.6746006555988,-1.77274958764284,-0.112393424764536));
#6075=CARTESIAN_POINT('Ctrl Pts',(92.6772946626731,-1.76991545896634,-0.151985751520627));
#6076=CARTESIAN_POINT('Ctrl Pts',(92.6790233757145,-1.76757863036,-0.177104692319194));
#6077=CARTESIAN_POINT('Ctrl Pts',(92.6902838227045,-1.74905353911342,-0.338811670470226));
#6078=CARTESIAN_POINT('Ctrl Pts',(92.700300299322,-1.71758321673294,-0.473155277589021));
#6079=CARTESIAN_POINT('Ctrl Pts',(92.7148508139103,-1.65008157532417,-0.660362602074984));
#6080=CARTESIAN_POINT('Ctrl Pts',(92.7193374353437,-1.62622339631619,-0.717109664540585));
#6081=CARTESIAN_POINT('Ctrl Pts',(92.7261522728757,-1.58473239674092,-0.80301633596489));
#6082=CARTESIAN_POINT('Ctrl Pts',(92.7285429440067,-1.56912602398888,-0.833100161945485));
#6083=CARTESIAN_POINT('Ctrl Pts',(92.7316607551414,-1.5472464559242,-0.872477528823854));
#6084=CARTESIAN_POINT('Ctrl Pts',(92.7324282416505,-1.54173349499317,-0.882182793020596));
#6085=CARTESIAN_POINT('Ctrl Pts',(92.7336927839779,-1.53243206937843,-0.89820389528087));
#6086=CARTESIAN_POINT('Ctrl Pts',(92.7341929820825,-1.52869522052787,-0.904549177455522));
#6087=CARTESIAN_POINT('Ctrl Pts',(92.7352062710777,-1.52100521738175,-0.917423259425176));
#6088=CARTESIAN_POINT('Ctrl Pts',(92.7357191748343,-1.51704926073363,-0.923950136253548));
#6089=CARTESIAN_POINT('Ctrl Pts',(92.7370598254484,-1.50654568553652,-0.941030498096524));
#6090=CARTESIAN_POINT('Ctrl Pts',(92.7378832328774,-1.49992910649765,-0.951541380102056));
#6091=CARTESIAN_POINT('Ctrl Pts',(92.7415219872807,-1.469979318751,-0.998029863197726));
#6092=CARTESIAN_POINT('Ctrl Pts',(92.7442688029124,-1.44545620347339,-1.03322786521234));
#6093=CARTESIAN_POINT('Ctrl Pts',(92.7555152196971,-1.33824239732307,-1.17581190044576));
#6094=CARTESIAN_POINT('Ctrl Pts',(92.7636216677633,-1.24467545659362,-1.27444640557481));
#6095=CARTESIAN_POINT('Ctrl Pts',(92.7760144671006,-1.09258281290789,-1.40188574127089));
#6096=CARTESIAN_POINT('Ctrl Pts',(92.7800049738278,-1.0422607701702,-1.43969165025828));
#6097=CARTESIAN_POINT('Ctrl Pts',(92.7853902078503,-0.973565239913303,-1.48580910498352));
#6098=CARTESIAN_POINT('Ctrl Pts',(92.7866916361762,-0.956903272501679,-1.4965941493721));
#6099=CARTESIAN_POINT('Ctrl Pts',(92.788876208919,-0.928860779391038,-1.51408588928242));
#6100=CARTESIAN_POINT('Ctrl Pts',(92.7897535146276,-0.917579621045383,-1.52094906247328));
#6101=CARTESIAN_POINT('Ctrl Pts',(92.7914886556546,-0.895236858220022,-1.53420279096481));
#6102=CARTESIAN_POINT('Ctrl Pts',(92.7923461417386,-0.884180746007873,-1.54060106118081));
#6103=CARTESIAN_POINT('Ctrl Pts',(92.7942475062959,-0.859639328325736,-1.55445220728275));
#6104=CARTESIAN_POINT('Ctrl Pts',(92.7952932825241,-0.846124247725795,-1.56184991941853));
#6105=CARTESIAN_POINT('Ctrl Pts',(92.798955337192,-0.798751502935135,-1.58698487436863));
#6106=CARTESIAN_POINT('Ctrl Pts',(92.8016031939177,-0.764421013818563,-1.60380331742119));
#6107=CARTESIAN_POINT('Ctrl Pts',(92.8133738097908,-0.611553288329752,-1.67266947766562));
#6108=CARTESIAN_POINT('Ctrl Pts',(92.8228685654091,-0.488084820807003,-1.71277101390206));
#6109=CARTESIAN_POINT('Ctrl Pts',(92.8375011641981,-0.291813139110086,-1.75355573015371));
#6110=CARTESIAN_POINT('Ctrl Pts',(92.8426510358254,-0.221434373987975,-1.76382577436859));
#6111=CARTESIAN_POINT('Ctrl Pts',(92.8488633136582,-0.133105667517972,-1.77134300593023));
#6112=CARTESIAN_POINT('Ctrl Pts',(92.8500845265591,-0.115565717665967,-1.77257377467411));
#6113=CARTESIAN_POINT('Ctrl Pts',(92.8518909360196,-0.0893148708898787,
-1.77402444886132));
#6114=CARTESIAN_POINT('Ctrl Pts',(92.8524860078789,-0.0806165145990328,
-1.77444100407357));
#6115=CARTESIAN_POINT('Ctrl Pts',(92.8535091260019,-0.0655671513773256,
-1.77505080921174));
#6116=CARTESIAN_POINT('Ctrl Pts',(92.8539387730379,-0.0592178169983456,
-1.77527397327142));
#6117=CARTESIAN_POINT('Ctrl Pts',(92.8549487071626,-0.0442234059140566,
-1.77572045444784));
#6118=CARTESIAN_POINT('Ctrl Pts',(92.855527385033,-0.0355777341403585,-1.77591471490798));
#6119=CARTESIAN_POINT('Ctrl Pts',(92.8572520826953,-0.00966083257458799,
-1.77630770135782));
#6120=CARTESIAN_POINT('Ctrl Pts',(92.8583883024626,0.00761279225494029,
-1.77631767472473));
#6121=CARTESIAN_POINT('Ctrl Pts',(92.86653258003,0.132619545578985,-1.77456620537457));
#6122=CARTESIAN_POINT('Ctrl Pts',(92.8731165972371,0.240008591932103,-1.76325698748452));
#6123=CARTESIAN_POINT('Ctrl Pts',(92.8821534255,0.384422170338835,-1.73460092324287));
#6124=CARTESIAN_POINT('Ctrl Pts',(92.8845754883257,0.422855596923087,-1.72563432677218));
#6125=CARTESIAN_POINT('Ctrl Pts',(92.8904142863441,0.514030905315646,-1.70113386405873));
#6126=CARTESIAN_POINT('Ctrl Pts',(92.8938453141875,0.566410003937744,-1.68441777622951));
#6127=CARTESIAN_POINT('Ctrl Pts',(92.8997656804178,0.653591557548651,-1.6520681557862));
#6128=CARTESIAN_POINT('Ctrl Pts',(92.9022179913669,0.688819078532507,-1.6376932136476));
#6129=CARTESIAN_POINT('Ctrl Pts',(92.9058012086586,0.738810826708043,-1.61539519226944));
#6130=CARTESIAN_POINT('Ctrl Pts',(92.9069016064861,0.753968355934791,-1.60837643341001));
#6131=CARTESIAN_POINT('Ctrl Pts',(92.9088478377335,0.780420239781259,-1.59567168918139));
#6132=CARTESIAN_POINT('Ctrl Pts',(92.9096904685797,0.79175722852988,-1.59007684318077));
#6133=CARTESIAN_POINT('Ctrl Pts',(92.9114597920135,0.815315333711167,-1.57813642326924));
#6134=CARTESIAN_POINT('Ctrl Pts',(92.912387216655,0.827524271661795,-1.57176882048247));
#6135=CARTESIAN_POINT('Ctrl Pts',(92.9148481840782,0.859546591391078,-1.55459098129583));
#6136=CARTESIAN_POINT('Ctrl Pts',(92.9163900352327,0.879229531531933,-1.54354423676119));
#6137=CARTESIAN_POINT('Ctrl Pts',(92.9248754401273,0.985450544687864,-1.48123839899402));
#6138=CARTESIAN_POINT('Ctrl Pts',(92.9320681726743,1.06771204575358,-1.42308289105365));
#6139=CARTESIAN_POINT('Ctrl Pts',(92.9447646069896,1.20108617267584,-1.3106915638036));
#6140=CARTESIAN_POINT('Ctrl Pts',(92.9501936567461,1.25454713468574,-1.25961573684614));
#6141=CARTESIAN_POINT('Ctrl Pts',(92.9598962218267,1.34522951642781,-1.16146180282468));
#6142=CARTESIAN_POINT('Ctrl Pts',(92.9641854274155,1.38354927611218,-1.11553971861347));
#6143=CARTESIAN_POINT('Ctrl Pts',(92.9692602804409,1.42742427844582,-1.05721259236665));
#6144=CARTESIAN_POINT('Ctrl Pts',(92.9701720244142,1.43524690480812,-1.04656814613235));
#6145=CARTESIAN_POINT('Ctrl Pts',(92.9716101838399,1.44750095043408,-1.02949791328233));
#6146=CARTESIAN_POINT('Ctrl Pts',(92.9721415668433,1.45200984371182,-1.02312871851253));
#6147=CARTESIAN_POINT('Ctrl Pts',(92.9731559433584,1.46058343567568,-1.01084695361096));
#6148=CARTESIAN_POINT('Ctrl Pts',(92.9736393323113,1.4646544827768,-1.00493919428011));
#6149=CARTESIAN_POINT('Ctrl Pts',(92.9747147103402,1.47367541374086,-0.991677074690893));
#6150=CARTESIAN_POINT('Ctrl Pts',(92.9753054572041,1.47860633269386,-0.984309893588972));
#6151=CARTESIAN_POINT('Ctrl Pts',(92.9773833078538,1.49585248192924,-0.958120726478997));
#6152=CARTESIAN_POINT('Ctrl Pts',(92.9788521920085,1.50786571471827,-0.939101205229439));
#6153=CARTESIAN_POINT('Ctrl Pts',(92.9886090336211,1.58614626039876,-0.809789372513874));
#6154=CARTESIAN_POINT('Ctrl Pts',(92.996351921846,1.64062870818219,-0.692794488604774));
#6155=CARTESIAN_POINT('Ctrl Pts',(93.0094907831567,1.70913289062676,-0.490976106703148));
#6156=CARTESIAN_POINT('Ctrl Pts',(93.014756121613,1.73053336059814,-0.409200099982136));
#6157=CARTESIAN_POINT('Ctrl Pts',(93.0218643634416,1.75076118881186,-0.300933470738367));
#6158=CARTESIAN_POINT('Ctrl Pts',(93.0235399162205,1.75493522141452,-0.275550273559126));
#6159=CARTESIAN_POINT('Ctrl Pts',(93.0261822486872,1.76058766833873,-0.235803422187769));
#6160=CARTESIAN_POINT('Ctrl Pts',(93.0271370818637,1.7624447312373,-0.221496592505313));
#6161=CARTESIAN_POINT('Ctrl Pts',(93.0289308379924,1.76558742425185,-0.194735308690751));
#6162=CARTESIAN_POINT('Ctrl Pts',(93.0297683470956,1.7669160494045,-0.182286734644646));
#6163=CARTESIAN_POINT('Ctrl Pts',(93.0316562258704,1.76960065690939,-0.154336330564025));
#6164=CARTESIAN_POINT('Ctrl Pts',(93.0327087908997,1.77088472937446,-0.138828801814831));
#6165=CARTESIAN_POINT('Ctrl Pts',(93.0354350894068,1.77366549006005,-0.0988682382603739));
#6166=CARTESIAN_POINT('Ctrl Pts',(93.0371180501293,1.77486027676062,-0.0743982061153983));
#6167=CARTESIAN_POINT('Ctrl Pts',(93.0388710464405,1.77557080561487,-0.0491223100769542));
#6168=CARTESIAN_POINT('Ctrl Pts',(93.0389258516589,1.77559248579042,-0.0483323025080003));
#6169=CARTESIAN_POINT('Ctrl Pts',(93.0389806716277,1.77561363837854,-0.0475422938458683));
#6170=CARTESIAN_POINT('Origin',(88.3562164250559,0.,0.));
#6171=CARTESIAN_POINT('',(93.938045236354,1.77561363622783,-0.0475423741708462));
#6172=CARTESIAN_POINT('',(93.7915308013958,1.77561364010973,-0.0475422291890938));
#6173=CARTESIAN_POINT('',(88.3562164250559,1.77561363837197,-0.0475422940912398));
#6174=CARTESIAN_POINT('',(93.3790868291138,3.82645600525644E-5,1.77624999958785));
#6175=CARTESIAN_POINT('Ctrl Pts',(93.938045236354,1.77561363622783,-0.0475423741708462));
#6176=CARTESIAN_POINT('Ctrl Pts',(93.9320040216653,1.77340196817429,-0.130143801279928));
#6177=CARTESIAN_POINT('Ctrl Pts',(93.9259827141224,1.76542829118073,-0.212520978178856));
#6178=CARTESIAN_POINT('Ctrl Pts',(93.9189430774626,1.74880132298718,-0.311564728677188));
#6179=CARTESIAN_POINT('Ctrl Pts',(93.9177108384249,1.74560292013426,-0.329012389570148));
#6180=CARTESIAN_POINT('Ctrl Pts',(93.9158914723543,1.74043938351934,-0.354980524151267));
#6181=CARTESIAN_POINT('Ctrl Pts',(93.9152942701028,1.73867194715723,-0.363538565386476));
#6182=CARTESIAN_POINT('Ctrl Pts',(93.9142211954599,1.73536307937548,-0.378983967867905));
#6183=CARTESIAN_POINT('Ctrl Pts',(93.9137441574733,1.73384369704369,-0.385875502480605));
#6184=CARTESIAN_POINT('Ctrl Pts',(93.9126651008141,1.73029650687055,-0.401520593850451));
#6185=CARTESIAN_POINT('Ctrl Pts',(93.9120645188153,1.72824331213126,-0.410268024280801));
#6186=CARTESIAN_POINT('Ctrl Pts',(93.9102023132568,1.72163309880907,-0.437499655893678));
#6187=CARTESIAN_POINT('Ctrl Pts',(93.9089529366966,1.71684507731633,-0.455927108119867));
#6188=CARTESIAN_POINT('Ctrl Pts',(93.9059971615295,1.70469268330158,-0.499787745425835));
#6189=CARTESIAN_POINT('Ctrl Pts',(93.9043032002053,1.69705400952092,-0.525140715300347));
#6190=CARTESIAN_POINT('Ctrl Pts',(93.8976356766913,1.66442135475245,-0.625286486790069));
#6191=CARTESIAN_POINT('Ctrl Pts',(93.8928080019055,1.63502490232017,-0.698553404615874));
#6192=CARTESIAN_POINT('Ctrl Pts',(93.8811612913827,1.55280905710831,-0.869565360747237));
#6193=CARTESIAN_POINT('Ctrl Pts',(93.8743435594647,1.49551655721073,-0.964772756437486));
#6194=CARTESIAN_POINT('Ctrl Pts',(93.8656231815207,1.41518924734116,-1.07373352421836));
#6195=CARTESIAN_POINT('Ctrl Pts',(93.8640310575246,1.40024560860681,-1.09314977429124));
#6196=CARTESIAN_POINT('Ctrl Pts',(93.8614022300274,1.37516165013015,-1.12438278616003));
#6197=CARTESIAN_POINT('Ctrl Pts',(93.860374909867,1.36525880250877,-1.13638663766106));
#6198=CARTESIAN_POINT('Ctrl Pts',(93.8585094737317,1.34710640653279,-1.15781049174282));
#6199=CARTESIAN_POINT('Ctrl Pts',(93.8576736701088,1.33891245749085,-1.16727641228749));
#6200=CARTESIAN_POINT('Ctrl Pts',(93.8558657023713,1.32106227848848,-1.18746227684354));
#6201=CARTESIAN_POINT('Ctrl Pts',(93.854892236438,1.31137418965857,-1.19815270973303));
#6202=CARTESIAN_POINT('Ctrl Pts',(93.852167665216,1.28405328395881,-1.22757194110003));
#6203=CARTESIAN_POINT('Ctrl Pts',(93.8504047869165,1.26614286407437,-1.24603685078672));
#6204=CARTESIAN_POINT('Ctrl Pts',(93.8427821983548,1.18774993255499,-1.32342099599285));
#6205=CARTESIAN_POINT('Ctrl Pts',(93.8367592011628,1.1235169424988,-1.37836828469259));
#6206=CARTESIAN_POINT('Ctrl Pts',(93.8212964989863,0.952147037806917,-1.50500371886784));
#6207=CARTESIAN_POINT('Ctrl Pts',(93.8117473829804,0.840662388396832,-1.57000265675587));
#6208=CARTESIAN_POINT('Ctrl Pts',(93.8010731118007,0.702582103987041,-1.63154793593117));
#6209=CARTESIAN_POINT('Ctrl Pts',(93.7995005288713,0.681858372751672,-1.64031690684089));
#6210=CARTESIAN_POINT('Ctrl Pts',(93.7973372793348,0.65274327787238,-1.65198937038501));
#6211=CARTESIAN_POINT('Ctrl Pts',(93.796729103392,0.644489271345008,-1.65522694941303));
#6212=CARTESIAN_POINT('Ctrl Pts',(93.7956352028668,0.629512374601053,-1.66097251948509));
#6213=CARTESIAN_POINT('Ctrl Pts',(93.7951482643689,0.622797877921894,-1.66350183377455));
#6214=CARTESIAN_POINT('Ctrl Pts',(93.7941369295977,0.608749083073824,-1.668696948887));
#6215=CARTESIAN_POINT('Ctrl Pts',(93.7936129674733,0.60141227312868,-1.67135520969737));
#6216=CARTESIAN_POINT('Ctrl Pts',(93.7922095065985,0.581611016536679,-1.67838229469115));
#6217=CARTESIAN_POINT('Ctrl Pts',(93.7913351096576,0.569114687547398,-1.68266069063211));
#6218=CARTESIAN_POINT('Ctrl Pts',(93.7865443292087,0.499845642432611,-1.70551649918976));
#6219=CARTESIAN_POINT('Ctrl Pts',(93.7827644038038,0.442205434573861,-1.72136228336056));
#6220=CARTESIAN_POINT('Ctrl Pts',(93.7744414191052,0.311726065367402,-1.75024304915061));
#6221=CARTESIAN_POINT('Ctrl Pts',(93.7699362214605,0.238653546971698,-1.76169492882366));
#6222=CARTESIAN_POINT('Ctrl Pts',(93.7592068748755,0.0649472156665822,-1.77790874772957));
#6223=CARTESIAN_POINT('Ctrl Pts',(93.7529613073609,-0.0357842304775489,
-1.77873368640014));
#6224=CARTESIAN_POINT('Ctrl Pts',(93.7449809601596,-0.158548078522177,-1.76930390121176));
#6225=CARTESIAN_POINT('Ctrl Pts',(93.74350540095,-0.181022977274753,-1.76714583281572));
#6226=CARTESIAN_POINT('Ctrl Pts',(93.7411082494639,-0.217130638805094,-1.76298270003029));
#6227=CARTESIAN_POINT('Ctrl Pts',(93.7401951249918,-0.230792296317716,-1.76124632371576));
#6228=CARTESIAN_POINT('Ctrl Pts',(93.738434051685,-0.256954154033847,-1.7576115767237));
#6229=CARTESIAN_POINT('Ctrl Pts',(93.7375869460015,-0.269457024522909,-1.75573824630454));
#6230=CARTESIAN_POINT('Ctrl Pts',(93.7356108454345,-0.298427873986478,-1.75108074952302));
#6231=CARTESIAN_POINT('Ctrl Pts',(93.7344787718251,-0.31487846980857,-1.74819750121955));
#6232=CARTESIAN_POINT('Ctrl Pts',(93.7307449589138,-0.36864215321565,-1.73799103540254));
#6233=CARTESIAN_POINT('Ctrl Pts',(93.7281130893119,-0.405758784505321,-1.7297020849127));
#6234=CARTESIAN_POINT('Ctrl Pts',(93.721593863067,-0.495768168326045,-1.70654457585489));
#6235=CARTESIAN_POINT('Ctrl Pts',(93.7176713089756,-0.548289936558882,-1.69040162929042));
#6236=CARTESIAN_POINT('Ctrl Pts',(93.7109035364631,-0.636404528595163,-1.65878006568367));
#6237=CARTESIAN_POINT('Ctrl Pts',(93.708084219214,-0.672395254245937,-1.64452013650389));
#6238=CARTESIAN_POINT('Ctrl Pts',(93.6973167712531,-0.807563790766749,-1.58578542617183));
#6239=CARTESIAN_POINT('Ctrl Pts',(93.6893190562768,-0.903059490742636,-1.53341513067342));
#6240=CARTESIAN_POINT('Ctrl Pts',(93.6805019194833,-1.0074357216936,-1.463021946694));
#6241=CARTESIAN_POINT('Ctrl Pts',(93.6793076720034,-1.02155711672744,-1.45319684214763));
#6242=CARTESIAN_POINT('Ctrl Pts',(93.6775329577856,-1.04254900703042,-1.43813426825716));
#6243=CARTESIAN_POINT('Ctrl Pts',(93.6769430978779,-1.04952721898671,-1.43304962581714));
#6244=CARTESIAN_POINT('Ctrl Pts',(93.6759251672233,-1.06157630512161,-1.42413489037724));
#6245=CARTESIAN_POINT('Ctrl Pts',(93.67549555619,-1.06666396515449,-1.42032828112927));
#6246=CARTESIAN_POINT('Ctrl Pts',(93.6744806943274,-1.07868764781347,-1.41123106262069));
#6247=CARTESIAN_POINT('Ctrl Pts',(93.6738971130666,-1.08560525780212,-1.40591656434271));
#6248=CARTESIAN_POINT('Ctrl Pts',(93.6721422362356,-1.10640654405852,-1.38969076356396));
#6249=CARTESIAN_POINT('Ctrl Pts',(93.6709812543199,-1.12016740256564,-1.37862282997714));
#6250=CARTESIAN_POINT('Ctrl Pts',(93.6651607267225,-1.18899510136212,-1.32155321326461));
#6251=CARTESIAN_POINT('Ctrl Pts',(93.6606817891378,-1.2414092592409,-1.27244550061471));
#6252=CARTESIAN_POINT('Ctrl Pts',(93.6481322897824,-1.38107371344113,-1.12472171908964));
#6253=CARTESIAN_POINT('Ctrl Pts',(93.64018721298,-1.46053336418497,-1.01941360888621));
#6254=CARTESIAN_POINT('Ctrl Pts',(93.629452946566,-1.54646306402993,-0.874572502762036));
#6255=CARTESIAN_POINT('Ctrl Pts',(93.6270726174005,-1.5642923033565,-0.842267390571588));
#6256=CARTESIAN_POINT('Ctrl Pts',(93.6235871731112,-1.58854659193674,-0.794890356955141));
#6257=CARTESIAN_POINT('Ctrl Pts',(93.622510641265,-1.5957900482274,-0.780246785797454));
#6258=CARTESIAN_POINT('Ctrl Pts',(93.6205892437427,-1.60827389349649,-0.754107877552704));
#6259=CARTESIAN_POINT('Ctrl Pts',(93.6197472674936,-1.61359563377497,-0.742652492098289));
#6260=CARTESIAN_POINT('Ctrl Pts',(93.6179758703421,-1.6244786988911,-0.718556683492309));
#6261=CARTESIAN_POINT('Ctrl Pts',(93.6170456812708,-1.63001567041215,-0.705906258640449));
#6262=CARTESIAN_POINT('Ctrl Pts',(93.6145691188102,-1.64428507611031,-0.672241385998971));
#6263=CARTESIAN_POINT('Ctrl Pts',(93.613014246432,-1.65276188417493,-0.651122079812201));
#6264=CARTESIAN_POINT('Ctrl Pts',(93.6095527734262,-1.67057024239244,-0.604163563689118));
#6265=CARTESIAN_POINT('Ctrl Pts',(93.6076404817285,-1.6797126333686,-0.57825934860139));
#6266=CARTESIAN_POINT('Ctrl Pts',(93.6015572786598,-1.70662140550392,-0.495983965454961));
#6267=CARTESIAN_POINT('Ctrl Pts',(93.5973239914352,-1.72217608872023,-0.438936328486937));
#6268=CARTESIAN_POINT('Ctrl Pts',(93.5846665985152,-1.7596541039577,-0.268383065021125));
#6269=CARTESIAN_POINT('Ctrl Pts',(93.5761140902391,-1.77338156229753,-0.153394345805444));
#6270=CARTESIAN_POINT('Ctrl Pts',(93.5653547064575,-1.77658990258446,-0.00301404823629758));
#6271=CARTESIAN_POINT('Ctrl Pts',(93.5628899757895,-1.77630657168885,0.0318764618742547));
#6272=CARTESIAN_POINT('Ctrl Pts',(93.5596680361613,-1.774559399598,0.0783447079826956));
#6273=CARTESIAN_POINT('Ctrl Pts',(93.5588686561726,-1.77400917811231,0.0899467069330056));
#6274=CARTESIAN_POINT('Ctrl Pts',(93.5576162994511,-1.77296102903341,0.108251589740391));
#6275=CARTESIAN_POINT('Ctrl Pts',(93.5571593327062,-1.77253880812099,0.114958230110525));
#6276=CARTESIAN_POINT('Ctrl Pts',(93.5562075753711,-1.77157561560948,0.128987642825595));
#6277=CARTESIAN_POINT('Ctrl Pts',(93.5557132402909,-1.77102728244535,0.136309726393413));
#6278=CARTESIAN_POINT('Ctrl Pts',(93.5544808293402,-1.76953970340671,0.154646361069168));
#6279=CARTESIAN_POINT('Ctrl Pts',(93.5537458725701,-1.76854298921556,0.165656179447372));
#6280=CARTESIAN_POINT('Ctrl Pts',(93.5508397881039,-1.76416570170394,0.209450866852258));
#6281=CARTESIAN_POINT('Ctrl Pts',(93.5487088337633,-1.75997552144474,0.242150319740251));
#6282=CARTESIAN_POINT('Ctrl Pts',(93.5428621565831,-1.74578335828127,0.332809238409397));
#6283=CARTESIAN_POINT('Ctrl Pts',(93.5392166058674,-1.73380960088183,0.390418678743127));
#6284=CARTESIAN_POINT('Ctrl Pts',(93.5268157923828,-1.6830938510655,0.58530846024065));
#6285=CARTESIAN_POINT('Ctrl Pts',(93.5181791435398,-1.63071217137066,0.71844605225803));
#6286=CARTESIAN_POINT('Ctrl Pts',(93.5073803504127,-1.55130555524469,0.865516791338427));
#6287=CARTESIAN_POINT('Ctrl Pts',(93.5057779949659,-1.5391804827255,0.886899987323495));
#6288=CARTESIAN_POINT('Ctrl Pts',(93.5032165485324,-1.51929128506586,0.920338720983961));
#6289=CARTESIAN_POINT('Ctrl Pts',(93.502267971553,-1.51181792878284,0.932564153379881));
#6290=CARTESIAN_POINT('Ctrl Pts',(93.5004876003179,-1.49759709416095,0.955207322603171));
#6291=CARTESIAN_POINT('Ctrl Pts',(93.4996572158886,-1.49088670474775,0.96564740236655));
#6292=CARTESIAN_POINT('Ctrl Pts',(93.4977710677138,-1.47547387399292,0.989083166695137));
#6293=CARTESIAN_POINT('Ctrl Pts',(93.4967129711615,-1.46670818130958,1.0020358012658));
#6294=CARTESIAN_POINT('Ctrl Pts',(93.4934754822273,-1.43953490224797,1.04106783774419));
#6295=CARTESIAN_POINT('Ctrl Pts',(93.4912760415947,-1.42059521647486,1.06676706908511));
#6296=CARTESIAN_POINT('Ctrl Pts',(93.4834010547684,-1.35114595929353,1.15587139016386));
#6297=CARTESIAN_POINT('Ctrl Pts',(93.477590588653,-1.29700616966977,1.21630838152252));
#6298=CARTESIAN_POINT('Ctrl Pts',(93.4646098790515,-1.16909880101702,1.34080956590284));
#6299=CARTESIAN_POINT('Ctrl Pts',(93.4574212913631,-1.0937855026046,1.4029240500182));
#6300=CARTESIAN_POINT('Ctrl Pts',(93.447431567054,-0.979698571696433,1.48221965593684));
#6301=CARTESIAN_POINT('Ctrl Pts',(93.4444868008816,-0.944818467454322,1.50469367654985));
#6302=CARTESIAN_POINT('Ctrl Pts',(93.4407546436979,-0.898616901716072,1.53222156787718));
#6303=CARTESIAN_POINT('Ctrl Pts',(93.4399072166342,-0.887987771924987,1.53840599561718));
#6304=CARTESIAN_POINT('Ctrl Pts',(93.43854652272,-0.870681856791702,1.54823609610075));
#6305=CARTESIAN_POINT('Ctrl Pts',(93.4380291376247,-0.864044592340077,1.55195001626316));
#6306=CARTESIAN_POINT('Ctrl Pts',(93.4370148880427,-0.850916603994066,1.5591855311238));
#6307=CARTESIAN_POINT('Ctrl Pts',(93.4365178964449,-0.844427428477376,1.5627094768021));
#6308=CARTESIAN_POINT('Ctrl Pts',(93.4352692836025,-0.827987626292969,1.57150480404216));
#6309=CARTESIAN_POINT('Ctrl Pts',(93.4345209589256,-0.818008285627792,1.5767223342951));
#6310=CARTESIAN_POINT('Ctrl Pts',(93.4314840568817,-0.777025429479143,1.59765568726248));
#6311=CARTESIAN_POINT('Ctrl Pts',(93.4292403758418,-0.745611308637735,1.612555848503));
#6312=CARTESIAN_POINT('Ctrl Pts',(93.4229490148593,-0.655011100536116,1.6523144714842));
#6313=CARTESIAN_POINT('Ctrl Pts',(93.4189849535115,-0.594885739416275,1.67490141431019));
#6314=CARTESIAN_POINT('Ctrl Pts',(93.4069910764914,-0.408801994032356,1.73351753081802));
#6315=CARTESIAN_POINT('Ctrl Pts',(93.3990256278216,-0.279986124400423,1.75892182844338));
#6316=CARTESIAN_POINT('Ctrl Pts',(93.3888759361916,-0.122991419722221,1.77218727789034));
#6317=CARTESIAN_POINT('Ctrl Pts',(93.3871422672075,-0.0963835139330152,
1.77383334469483));
#6318=CARTESIAN_POINT('Ctrl Pts',(93.3844889443492,-0.0560514774909538,
1.77541832429632));
#6319=CARTESIAN_POINT('Ctrl Pts',(93.3835829948779,-0.0423477859082393,
1.77579802955084));
#6320=CARTESIAN_POINT('Ctrl Pts',(93.3820343143278,-0.0190449371209913,
1.77617382839407));
#6321=CARTESIAN_POINT('Ctrl Pts',(93.3813941425469,-0.00944758569584646,
1.77625080269604));
#6322=CARTESIAN_POINT('Ctrl Pts',(93.3807515265229,0.000149729197527163,
1.77624999368928));
#6323=CARTESIAN_POINT('Ctrl Pts',(93.1883366943682,1.77561363837197,-0.0475422940912359));
#6324=CARTESIAN_POINT('Ctrl Pts',(93.1925001087569,1.77726738439512,0.0142219528650102));
#6325=CARTESIAN_POINT('Ctrl Pts',(93.1966635231455,1.77569212163206,0.0759763082135405));
#6326=CARTESIAN_POINT('Ctrl Pts',(93.2008269375341,1.77093077259767,0.13736178932519));
#6327=CARTESIAN_POINT('Ctrl Pts',(93.205125747123,1.7660145833899,0.200743540500161));
#6328=CARTESIAN_POINT('Ctrl Pts',(93.2094245567119,1.75768143007869,0.263990072622322));
#6329=CARTESIAN_POINT('Ctrl Pts',(93.2137233663007,1.74594638510628,0.326703662107288));
#6330=CARTESIAN_POINT('Ctrl Pts',(93.2181506282696,1.73386068620864,0.391291191263542));
#6331=CARTESIAN_POINT('Ctrl Pts',(93.2225778902384,1.71816647917446,0.45531287608599));
#6332=CARTESIAN_POINT('Ctrl Pts',(93.2270051522073,1.69893806927726,0.518337244716658));
#6333=CARTESIAN_POINT('Ctrl Pts',(93.2312921458582,1.68031887038518,0.579364821144228));
#6334=CARTESIAN_POINT('Ctrl Pts',(93.235579139509,1.65838623789395,0.639456812182291));
#6335=CARTESIAN_POINT('Ctrl Pts',(93.2398661331599,1.63325941068488,0.698231881189398));
#6336=CARTESIAN_POINT('Ctrl Pts',(93.2441505065298,1.60814794140566,0.756971025908113));
#6337=CARTESIAN_POINT('Ctrl Pts',(93.2484348798996,1.57984634677411,0.814394382467918));
#6338=CARTESIAN_POINT('Ctrl Pts',(93.2527192532695,1.54852263283247,0.870138907362264));
#6339=CARTESIAN_POINT('Ctrl Pts',(93.2570025501981,1.51720678891874,0.925869426543002));
#6340=CARTESIAN_POINT('Ctrl Pts',(93.2612858471267,1.48287057976837,0.979921512287453));
#6341=CARTESIAN_POINT('Ctrl Pts',(93.2655691440553,1.44572785001253,1.03195690132784));
#6342=CARTESIAN_POINT('Ctrl Pts',(93.269852906609,1.40858108257572,1.08399794698801));
#6343=CARTESIAN_POINT('Ctrl Pts',(93.2741366691627,1.36862748439017,1.13402145265898));
#6344=CARTESIAN_POINT('Ctrl Pts',(93.2784204317164,1.32612293023111,1.18171994838679));
#6345=CARTESIAN_POINT('Ctrl Pts',(93.282708952196,1.28357116675154,1.22947142228638));
#6346=CARTESIAN_POINT('Ctrl Pts',(93.2869974726756,1.23846313195367,1.27489235892395));
#6347=CARTESIAN_POINT('Ctrl Pts',(93.2912859931552,1.19109269473216,1.31771099071674));
#6348=CARTESIAN_POINT('Ctrl Pts',(93.2955773939946,1.14369044143279,1.36055838139382));
#6349=CARTESIAN_POINT('Ctrl Pts',(93.299868794834,1.0940231544451,1.40079967367227));
#6350=CARTESIAN_POINT('Ctrl Pts',(93.3041601956733,1.04241672098266,1.43820424221171));
#6351=CARTESIAN_POINT('Ctrl Pts',(93.3084588322712,0.990723273581195,1.47567187883449));
#6352=CARTESIAN_POINT('Ctrl Pts',(93.3127574688691,0.93708458160194,1.51029298062953));
#6353=CARTESIAN_POINT('Ctrl Pts',(93.317056105467,0.88185327564548,1.5418815981564));
#6354=CARTESIAN_POINT('Ctrl Pts',(93.3180299548291,0.869340710126261,1.54903794978745));
#6355=CARTESIAN_POINT('Ctrl Pts',(93.3190038041912,0.856746490809696,1.55603885512491));
#6356=CARTESIAN_POINT('Ctrl Pts',(93.3199776535533,0.844074858812542,1.56288249565365));
#6357=CARTESIAN_POINT('Ctrl Pts',(93.3245053479899,0.785160944681927,1.59470046910347));
#6358=CARTESIAN_POINT('Ctrl Pts',(93.3290330424265,0.724353261935751,1.62323346819936));
#6359=CARTESIAN_POINT('Ctrl Pts',(93.333560736863,0.662032291516035,1.64826493850049));
#6360=CARTESIAN_POINT('Ctrl Pts',(93.3380747387602,0.599899790604014,1.67322070926015));
#6361=CARTESIAN_POINT('Ctrl Pts',(93.3425887406574,0.536263505898929,1.69469587559583));
#6362=CARTESIAN_POINT('Ctrl Pts',(93.3471027425546,0.471526535092008,1.71252059526422));
#6363=CARTESIAN_POINT('Ctrl Pts',(93.3516083627061,0.406909769999983,1.73031221741286));
#6364=CARTESIAN_POINT('Ctrl Pts',(93.3561139828576,0.341196788975856,1.74446675420195));
#6365=CARTESIAN_POINT('Ctrl Pts',(93.3606196030091,0.274808832373806,1.7548630055219));
#6366=CARTESIAN_POINT('Ctrl Pts',(93.3651149452393,0.208572315568176,1.76523554160397));
#6367=CARTESIAN_POINT('Ctrl Pts',(93.3696102874694,0.141664306510061,1.77186679104811));
#6368=CARTESIAN_POINT('Ctrl Pts',(93.3741056296996,0.074517532603036,1.77468622574098));
#6369=CARTESIAN_POINT('Ctrl Pts',(93.3757660295043,0.0497161972259653,1.77572761226371));
#6370=CARTESIAN_POINT('Ctrl Pts',(93.3774264293091,0.0248823982268752,1.77624946438737));
#6371=CARTESIAN_POINT('Ctrl Pts',(93.3790868291138,3.82645600525644E-5,
1.77624999958785));
#6372=CARTESIAN_POINT('Ctrl Pts',(93.0389806716277,1.77561363837854,-0.0475422938458682));
#6373=CARTESIAN_POINT('Ctrl Pts',(93.0466237494881,1.77856276223817,0.0626018351563203));
#6374=CARTESIAN_POINT('Ctrl Pts',(93.0545765376933,1.77125660689251,0.172765614818531));
#6375=CARTESIAN_POINT('Ctrl Pts',(93.068382024661,1.74130926464116,0.359325238365741));
#6376=CARTESIAN_POINT('Ctrl Pts',(93.0741668361496,1.72365754904715,0.436208821378193));
#6377=CARTESIAN_POINT('Ctrl Pts',(93.0817185902019,1.69333538960863,0.537009883556233));
#6378=CARTESIAN_POINT('Ctrl Pts',(93.0836009048678,1.68514662888125,0.562179103241644));
#6379=CARTESIAN_POINT('Ctrl Pts',(93.0867963251137,1.67010711882088,0.605118550747016));
#6380=CARTESIAN_POINT('Ctrl Pts',(93.0881205895987,1.66352758768491,0.62297856036129));
#6381=CARTESIAN_POINT('Ctrl Pts',(93.0900474752986,1.6534214197674,0.649108907844275));
#6382=CARTESIAN_POINT('Ctrl Pts',(93.0906619087197,1.65011728296532,0.657463099214146));
#6383=CARTESIAN_POINT('Ctrl Pts',(93.0917523113015,1.64410472969126,0.672334364873515));
#6384=CARTESIAN_POINT('Ctrl Pts',(93.0922296507737,1.64142070206472,0.678860769387451));
#6385=CARTESIAN_POINT('Ctrl Pts',(93.0932928280349,1.63532580289314,0.693433448442733));
#6386=CARTESIAN_POINT('Ctrl Pts',(93.0938774328868,1.63189437433871,0.701470732161606));
#6387=CARTESIAN_POINT('Ctrl Pts',(93.0956387291118,1.62131778469842,0.725746109868362));
#6388=CARTESIAN_POINT('Ctrl Pts',(93.0968049954689,1.61398831044527,0.741903341082248));
#6389=CARTESIAN_POINT('Ctrl Pts',(93.1047041262956,1.56220333582018,0.851657850319834));
#6390=CARTESIAN_POINT('Ctrl Pts',(93.1110490402436,1.50986815566692,0.941331004573779));
#6391=CARTESIAN_POINT('Ctrl Pts',(93.1200228189697,1.4254240247358,1.06067981485194));
#6392=CARTESIAN_POINT('Ctrl Pts',(93.1226336321318,1.39960222412412,1.09452676607996));
#6393=CARTESIAN_POINT('Ctrl Pts',(93.1286739926768,1.33760416451959,1.17000746062796));
#6394=CARTESIAN_POINT('Ctrl Pts',(93.1321148882407,1.3006567244868,1.21094747294155));
#6395=CARTESIAN_POINT('Ctrl Pts',(93.1380503393777,1.2350399161863,1.27718187378748));
#6396=CARTESIAN_POINT('Ctrl Pts',(93.1405076003237,1.20734906293717,1.30338982700217));
#6397=CARTESIAN_POINT('Ctrl Pts',(93.1440967365837,1.16633388764828,1.33977936901729));
#6398=CARTESIAN_POINT('Ctrl Pts',(93.1451979582635,1.15367405164561,1.35069598579465));
#6399=CARTESIAN_POINT('Ctrl Pts',(93.1471451291475,1.13117113455504,1.36955313878082));
#6400=CARTESIAN_POINT('Ctrl Pts',(93.1479878656392,1.12139367336679,1.37757037960178));
#6401=CARTESIAN_POINT('Ctrl Pts',(93.1497568955079,1.10079583096589,1.39409542129661));
#6402=CARTESIAN_POINT('Ctrl Pts',(93.1506839155591,1.08996052049543,1.40258317055842));
#6403=CARTESIAN_POINT('Ctrl Pts',(93.1531425857835,1.06112159496285,1.42463791358823));
#6404=CARTESIAN_POINT('Ctrl Pts',(93.1546825163166,1.04295696024656,1.43798919382491));
#6405=CARTESIAN_POINT('Ctrl Pts',(93.1631519334932,0.942546572237878,1.5088889249118));
#6406=CARTESIAN_POINT('Ctrl Pts',(93.1703295816794,0.855802658799709,1.55972293240777));
#6407=CARTESIAN_POINT('Ctrl Pts',(93.1829456264651,0.699390325727027,1.63439359383794));
#6408=CARTESIAN_POINT('Ctrl Pts',(93.1883083752161,0.631661842850541,1.66174381072569));
#6409=CARTESIAN_POINT('Ctrl Pts',(93.1965977045116,0.523415087176101,1.69787916630162));
#6410=CARTESIAN_POINT('Ctrl Pts',(93.1995634411815,0.483943349750302,1.70954855634834));
#6411=CARTESIAN_POINT('Ctrl Pts',(93.2043298501154,0.418829790881935,1.72636230725136));
#6412=CARTESIAN_POINT('Ctrl Pts',(93.2061592774517,0.39341747326498,1.73233024449381));
#6413=CARTESIAN_POINT('Ctrl Pts',(93.2086617840972,0.357949607195601,1.73983884321208));
#6414=CARTESIAN_POINT('Ctrl Pts',(93.2093583023446,0.347999775919662,1.74185627707938));
#6415=CARTESIAN_POINT('Ctrl Pts',(93.2105393151326,0.330985775916135,1.74515443636864));
#6416=CARTESIAN_POINT('Ctrl Pts',(93.2110261277689,0.323930248719547,1.74647782473955));
#6417=CARTESIAN_POINT('Ctrl Pts',(93.2120494716762,0.309005802074096,1.74918360935026));
#6418=CARTESIAN_POINT('Ctrl Pts',(93.2125854386499,0.301135333264894,1.75055574097804));
#6419=CARTESIAN_POINT('Ctrl Pts',(93.2140575032005,0.279378771753651,1.75419768812772));
#6420=CARTESIAN_POINT('Ctrl Pts',(93.214987610092,0.265474211724137,1.75635574435876));
#6421=CARTESIAN_POINT('Ctrl Pts',(93.2213928145935,0.168751189816154,1.77019269873321));
#6422=CARTESIAN_POINT('Ctrl Pts',(93.2265983032021,0.0852129682182508,1.77617609730427));
#6423=CARTESIAN_POINT('Ctrl Pts',(93.2407250864887,-0.144055467551346,1.77637676561385));
#6424=CARTESIAN_POINT('Ctrl Pts',(93.2495338211782,-0.289113125374711,1.75860060391683));
#6425=CARTESIAN_POINT('Ctrl Pts',(93.2605080780151,-0.4538127190016,1.71746960217272));
#6426=CARTESIAN_POINT('Ctrl Pts',(93.2620838103519,-0.477130983352542,1.71113814513665));
#6427=CARTESIAN_POINT('Ctrl Pts',(93.264612310666,-0.513972209549877,1.7003232964099));
#6428=CARTESIAN_POINT('Ctrl Pts',(93.2655550279725,-0.527583389219831,1.69614931301314));
#6429=CARTESIAN_POINT('Ctrl Pts',(93.2672547881802,-0.551892759826345,1.68837372453526));
#6430=CARTESIAN_POINT('Ctrl Pts',(93.2680097951912,-0.562609682777856,1.68483286611478));
#6431=CARTESIAN_POINT('Ctrl Pts',(93.2697910016446,-0.587698442062218,1.67627750860635));
#6432=CARTESIAN_POINT('Ctrl Pts',(93.2708199062474,-0.602040812719904,1.67117999607776));
#6433=CARTESIAN_POINT('Ctrl Pts',(93.2738750850129,-0.644175749433544,1.6555917661869));
#6434=CARTESIAN_POINT('Ctrl Pts',(93.275918225121,-0.671771467834419,1.64458791262244));
#6435=CARTESIAN_POINT('Ctrl Pts',(93.280695107706,-0.734925129995118,1.61755054030976));
#6436=CARTESIAN_POINT('Ctrl Pts',(93.2834437773362,-0.77025579586377,1.60102789692105));
#6437=CARTESIAN_POINT('Ctrl Pts',(93.2941859788216,-0.904557204985671,1.53274623472518));
#6438=CARTESIAN_POINT('Ctrl Pts',(93.3024022874923,-0.999101206697713,1.47286365211513));
#6439=CARTESIAN_POINT('Ctrl Pts',(93.3156278665941,-1.14261128187062,1.3617566443569));
#6440=CARTESIAN_POINT('Ctrl Pts',(93.3206690177548,-1.19527162885448,1.31577716091648));
#6441=CARTESIAN_POINT('Ctrl Pts',(93.3264999739985,-1.25499901315944,1.25707378632538));
#6442=CARTESIAN_POINT('Ctrl Pts',(93.3274598810676,-1.26479194367088,1.2472202678825));
#6443=CARTESIAN_POINT('Ctrl Pts',(93.3289559176588,-1.28000663913058,1.23154791946167));
#6444=CARTESIAN_POINT('Ctrl Pts',(93.3294976887397,-1.28550641137482,1.22580608038096));
#6445=CARTESIAN_POINT('Ctrl Pts',(93.330523869171,-1.29590785623306,1.21479982883754));
#6446=CARTESIAN_POINT('Ctrl Pts',(93.3310087594534,-1.3008163297648,1.20954234069556));
#6447=CARTESIAN_POINT('Ctrl Pts',(93.3321781411007,-1.31263466118435,1.19672851856032));
#6448=CARTESIAN_POINT('Ctrl Pts',(93.3328601930549,-1.31951149890743,1.18914184085805));
#6449=CARTESIAN_POINT('Ctrl Pts',(93.3353048740101,-1.34408221630503,1.16155926800799));
#6450=CARTESIAN_POINT('Ctrl Pts',(93.3370417718139,-1.36139125708832,1.1412234510216));
#6451=CARTESIAN_POINT('Ctrl Pts',(93.3414876257601,-1.40507187595266,1.08749564385176));
#6452=CARTESIAN_POINT('Ctrl Pts',(93.3441607592581,-1.43071480980057,1.05353184774018));
#6453=CARTESIAN_POINT('Ctrl Pts',(93.3546129212042,-1.52713830710726,0.915797181125603));
#6454=CARTESIAN_POINT('Ctrl Pts',(93.3621693425301,-1.58804692661192,0.805570345203826));
#6455=CARTESIAN_POINT('Ctrl Pts',(93.3733550079706,-1.65715815662269,0.641586219267288));
#6456=CARTESIAN_POINT('Ctrl Pts',(93.376695272091,-1.67534926650564,0.592461040548626));
#6457=CARTESIAN_POINT('Ctrl Pts',(93.3813605582293,-1.69722382044454,0.524276612993916));
#6458=CARTESIAN_POINT('Ctrl Pts',(93.3826238986236,-1.70280601142582,0.505852056916281));
#6459=CARTESIAN_POINT('Ctrl Pts',(93.3846759496079,-1.71131911804834,0.476014363890488));
#6460=CARTESIAN_POINT('Ctrl Pts',(93.3854585118966,-1.71443794937603,0.46465611455767));
#6461=CARTESIAN_POINT('Ctrl Pts',(93.3871002172263,-1.72071371056454,0.440877097683268));
#6462=CARTESIAN_POINT('Ctrl Pts',(93.3879599878179,-1.72384963068021,0.428451543188662));
#6463=CARTESIAN_POINT('Ctrl Pts',(93.3900243410106,-1.731018996276,0.398690436958075));
#6464=CARTESIAN_POINT('Ctrl Pts',(93.3912328771392,-1.73492679956393,0.381326356077841));
#6465=CARTESIAN_POINT('Ctrl Pts',(93.3955459623566,-1.74784996919096,0.319585661271104));
#6466=CARTESIAN_POINT('Ctrl Pts',(93.398695155381,-1.75542804394449,0.274929546853203));
#6467=CARTESIAN_POINT('Ctrl Pts',(93.406937362782,-1.770546130218,0.159176547786722));
#6468=CARTESIAN_POINT('Ctrl Pts',(93.4120961228154,-1.77551538882601,0.0878298788422582));
#6469=CARTESIAN_POINT('Ctrl Pts',(93.4255817991173,-1.77722167887632,-0.0971453400352781));
#6470=CARTESIAN_POINT('Ctrl Pts',(93.4339665626487,-1.76738188837031,-0.210518445142822));
#6471=CARTESIAN_POINT('Ctrl Pts',(93.4434999581633,-1.74286401574749,-0.343448354249441));
#6472=CARTESIAN_POINT('Ctrl Pts',(93.445010113681,-1.73855312700722,-0.364643493459479));
#6473=CARTESIAN_POINT('Ctrl Pts',(93.4471023568821,-1.73196136502418,-0.394271479965715));
#6474=CARTESIAN_POINT('Ctrl Pts',(93.4477005507389,-1.73000398653356,-0.402773365964168));
#6475=CARTESIAN_POINT('Ctrl Pts',(93.4487821202922,-1.72633057425892,-0.418207852105489));
#6476=CARTESIAN_POINT('Ctrl Pts',(93.4492666190073,-1.72463522216319,-0.425145171894172));
#6477=CARTESIAN_POINT('Ctrl Pts',(93.450280305827,-1.72098210251948,-0.439712065679702));
#6478=CARTESIAN_POINT('Ctrl Pts',(93.4508089853319,-1.7190153660746,-0.447339105302079));
#6479=CARTESIAN_POINT('Ctrl Pts',(93.4522393713453,-1.71352838647735,-0.468047030342525));
#6480=CARTESIAN_POINT('Ctrl Pts',(93.4531356340948,-1.7099090572664,-0.481101441839765));
#6481=CARTESIAN_POINT('Ctrl Pts',(93.4584283933487,-1.68747505807705,-0.558564504130073));
#6482=CARTESIAN_POINT('Ctrl Pts',(93.4626521376049,-1.66517018725408,-0.621913758129473));
#6483=CARTESIAN_POINT('Ctrl Pts',(93.4760225337471,-1.58217667853029,-0.820864970033614));
#6484=CARTESIAN_POINT('Ctrl Pts',(93.4849280538535,-1.5080766132944,-0.950161368031937));
#6485=CARTESIAN_POINT('Ctrl Pts',(93.4965570197942,-1.39869702116139,-1.09536396913253));
#6486=CARTESIAN_POINT('Ctrl Pts',(93.4987141172584,-1.37789269710149,-1.1214218959304));
#6487=CARTESIAN_POINT('Ctrl Pts',(93.5019425616299,-1.34610353782138,-1.15901772057991));
#6488=CARTESIAN_POINT('Ctrl Pts',(93.5029914300477,-1.33567633931577,-1.17101900086306));
#6489=CARTESIAN_POINT('Ctrl Pts',(93.504880058373,-1.31673426360768,-1.1922383842779));
#6490=CARTESIAN_POINT('Ctrl Pts',(93.5057172442871,-1.30828004865463,-1.20150937837215));
#6491=CARTESIAN_POINT('Ctrl Pts',(93.5075107369181,-1.29005145660743,-1.22107856956718));
#6492=CARTESIAN_POINT('Ctrl Pts',(93.5084681545735,-1.28025044974474,-1.23135064025902));
#6493=CARTESIAN_POINT('Ctrl Pts',(93.5111001692026,-1.25312363174504,-1.25910725599619));
#6494=CARTESIAN_POINT('Ctrl Pts',(93.5127852651667,-1.23555641318794,-1.27635032899491));
#6495=CARTESIAN_POINT('Ctrl Pts',(93.5218488338579,-1.14005899625464,-1.36626622226673));
#6496=CARTESIAN_POINT('Ctrl Pts',(93.5295048007982,-1.05607827440354,-1.43216956662259));
#6497=CARTESIAN_POINT('Ctrl Pts',(93.5459087231474,-0.867457826424393,-1.55453499842616));
#6498=CARTESIAN_POINT('Ctrl Pts',(93.554644472928,-0.762010315445193,-1.60885248446999));
#6499=CARTESIAN_POINT('Ctrl Pts',(93.5640575430095,-0.63682928793766,-1.65824496356577));
#6500=CARTESIAN_POINT('Ctrl Pts',(93.5651842445911,-0.621638060831142,-1.66399941979958));
#6501=CARTESIAN_POINT('Ctrl Pts',(93.5668863550844,-0.598338813046932,-1.67246157628475));
#6502=CARTESIAN_POINT('Ctrl Pts',(93.5674698869663,-0.59028709819039,-1.67532033017041));
#6503=CARTESIAN_POINT('Ctrl Pts',(93.5685252967295,-0.575601581414987,-1.68041538968882));
#6504=CARTESIAN_POINT('Ctrl Pts',(93.5689982214751,-0.568974956954876,-1.68267066415234));
#6505=CARTESIAN_POINT('Ctrl Pts',(93.5700857405124,-0.553631414401922,-1.68779160622621));
#6506=CARTESIAN_POINT('Ctrl Pts',(93.5706986989563,-0.544905417766542,-1.69062897880467));
#6507=CARTESIAN_POINT('Ctrl Pts',(93.5726417421401,-0.517011230177523,-1.69946073265534));
#6508=CARTESIAN_POINT('Ctrl Pts',(93.5739580130385,-0.497762445931506,-1.70519794290838));
#6509=CARTESIAN_POINT('Ctrl Pts',(93.5771055971458,-0.45100612753277,-1.71827466120828));
#6510=CARTESIAN_POINT('Ctrl Pts',(93.5789221977344,-0.423410869793095,-1.72528193366303));
#6511=CARTESIAN_POINT('Ctrl Pts',(93.5864529072088,-0.307103322391783,-1.7518569824724));
#6512=CARTESIAN_POINT('Ctrl Pts',(93.5919807602588,-0.217121954785275,-1.76526923050722));
#6513=CARTESIAN_POINT('Ctrl Pts',(93.6034323668234,-0.031289950246743,-1.77853790610811));
#6514=CARTESIAN_POINT('Ctrl Pts',(93.6093462555186,0.0643074665533043,-1.77764951328542));
#6515=CARTESIAN_POINT('Ctrl Pts',(93.6170688878634,0.183693455887243,-1.76689486791421));
#6516=CARTESIAN_POINT('Ctrl Pts',(93.6186564506637,0.207973532173791,-1.76420171106395));
#6517=CARTESIAN_POINT('Ctrl Pts',(93.6212792864363,0.247596116703773,-1.75897746360971));
#6518=CARTESIAN_POINT('Ctrl Pts',(93.622305249987,0.26297504176311,-1.75674404973668));
#6519=CARTESIAN_POINT('Ctrl Pts',(93.6241692168645,0.290685503937775,-1.75234776705317));
#6520=CARTESIAN_POINT('Ctrl Pts',(93.6250049240221,0.303027362236372,-1.75025574212245));
#6521=CARTESIAN_POINT('Ctrl Pts',(93.6268138063119,0.329558085912075,-1.74546959092179));
#6522=CARTESIAN_POINT('Ctrl Pts',(93.627788295605,0.343738184161768,-1.74273252797948));
#6523=CARTESIAN_POINT('Ctrl Pts',(93.6305189196209,0.383149258995308,-1.73462563824325));
#6524=CARTESIAN_POINT('Ctrl Pts',(93.6322869135237,0.408298102118649,-1.72887882671141));
#6525=CARTESIAN_POINT('Ctrl Pts',(93.6399524352542,0.515715186706416,-1.70185836465579));
#6526=CARTESIAN_POINT('Ctrl Pts',(93.646015449824,0.59651342424197,-1.67524688746557));
#6527=CARTESIAN_POINT('Ctrl Pts',(93.6617358188239,0.796845963813567,-1.5929308214231));
#6528=CARTESIAN_POINT('Ctrl Pts',(93.6715102805786,0.912666063389049,-1.52952104056577));
#6529=CARTESIAN_POINT('Ctrl Pts',(93.6820724513716,1.03551523099174,-1.44329915502099));
#6530=CARTESIAN_POINT('Ctrl Pts',(93.6833591176944,1.05044680101376,-1.43246843854411));
#6531=CARTESIAN_POINT('Ctrl Pts',(93.6852547382454,1.07243127297097,-1.41599318964344));
#6532=CARTESIAN_POINT('Ctrl Pts',(93.6858742416867,1.07961372362891,-1.41052464169013));
#6533=CARTESIAN_POINT('Ctrl Pts',(93.6869822492554,1.09246113672489,-1.40058729792259));
#6534=CARTESIAN_POINT('Ctrl Pts',(93.6874720699532,1.09814114573778,-1.39613829746063));
#6535=CARTESIAN_POINT('Ctrl Pts',(93.6884812926179,1.10984817240773,-1.38685284213382));
#6536=CARTESIAN_POINT('Ctrl Pts',(93.6890003402096,1.11587098882433,-1.38201147374414));
#6537=CARTESIAN_POINT('Ctrl Pts',(93.6903759192982,1.13183075071594,-1.36901005624242));
#6538=CARTESIAN_POINT('Ctrl Pts',(93.6912276931076,1.14171122872236,-1.36078098031617));
#6539=CARTESIAN_POINT('Ctrl Pts',(93.6955973104938,1.1923269147887,-1.31768565801692));
#6540=CARTESIAN_POINT('Ctrl Pts',(93.6990056079059,1.23156152335528,-1.28109186312229));
#6541=CARTESIAN_POINT('Ctrl Pts',(93.7131781827097,1.39013393825072,-1.11916259639066));
#6542=CARTESIAN_POINT('Ctrl Pts',(93.7234471422347,1.49247095608509,-0.978534931265175));
#6543=CARTESIAN_POINT('Ctrl Pts',(93.7361748205297,1.58428348972868,-0.803563249856688));
#6544=CARTESIAN_POINT('Ctrl Pts',(93.7377718249348,1.59524952152713,-0.781566978706564));
#6545=CARTESIAN_POINT('Ctrl Pts',(93.7404070213544,1.61241713724336,-0.74526362825554));
#6546=CARTESIAN_POINT('Ctrl Pts',(93.7414357501652,1.61889315340659,-0.731089482967122));
#6547=CARTESIAN_POINT('Ctrl Pts',(93.7433026555409,1.6302346246133,-0.705376425318109));
#6548=CARTESIAN_POINT('Ctrl Pts',(93.7441385023704,1.635166192292,-0.693867669271847));
#6549=CARTESIAN_POINT('Ctrl Pts',(93.7459453364531,1.64551086646122,-0.669003512251526));
#6550=CARTESIAN_POINT('Ctrl Pts',(93.7469176118721,1.65088390892722,-0.655632525840628));
#6551=CARTESIAN_POINT('Ctrl Pts',(93.7496353783921,1.6653640157855,-0.618291375512968));
#6552=CARTESIAN_POINT('Ctrl Pts',(93.7513925471767,1.67411530134087,-0.594187990619681));
#6553=CARTESIAN_POINT('Ctrl Pts',(93.7596819553197,1.71255342333467,-0.480719815585401));
#6554=CARTESIAN_POINT('Ctrl Pts',(93.7664229787929,1.73562130111621,-0.389287305957905));
#6555=CARTESIAN_POINT('Ctrl Pts',(93.7793509740582,1.76526961856507,-0.214146429622917));
#6556=CARTESIAN_POINT('Ctrl Pts',(93.7854943907676,1.77338001039965,-0.130964135309562));
#6557=CARTESIAN_POINT('Ctrl Pts',(93.7915308013958,1.77561364010973,-0.0475422291890938));
#6558=CARTESIAN_POINT('Origin',(88.3562164250559,0.,0.));
#6559=CARTESIAN_POINT('',(94.6900676319115,1.77561363837053,-0.0475422941449777));
#6560=CARTESIAN_POINT('',(94.5412649413994,1.77561364082572,-0.0475422024484503));
#6561=CARTESIAN_POINT('',(88.3562164250559,1.77561363837197,-0.0475422940912398));
#6562=CARTESIAN_POINT('Ctrl Pts',(94.6900676319115,1.77561363837053,-0.0475422941449777));
#6563=CARTESIAN_POINT('Ctrl Pts',(94.6893507188366,1.77532856922536,-0.0581890807830827));
#6564=CARTESIAN_POINT('Ctrl Pts',(94.6886308105993,1.77494775027251,-0.0688329602318011));
#6565=CARTESIAN_POINT('Ctrl Pts',(94.6861831815559,1.77333438493924,-0.104856300293904));
#6566=CARTESIAN_POINT('Ctrl Pts',(94.684441590984,1.77165305712317,-0.130211417406875));
#6567=CARTESIAN_POINT('Ctrl Pts',(94.672685378898,1.75677823088517,-0.299449024897515));
#6568=CARTESIAN_POINT('Ctrl Pts',(94.6621304716666,1.72661593432615,-0.441272503813269));
#6569=CARTESIAN_POINT('Ctrl Pts',(94.6455425341743,1.65275463930097,-0.655965845456816));
#6570=CARTESIAN_POINT('Ctrl Pts',(94.6395427093636,1.62045850308286,-0.732124515511155));
#6571=CARTESIAN_POINT('Ctrl Pts',(94.632811709424,1.57661523445818,-0.818257267904971));
#6572=CARTESIAN_POINT('Ctrl Pts',(94.6318428774882,1.57010851206846,-0.830674331617518));
#6573=CARTESIAN_POINT('Ctrl Pts',(94.6303361219136,1.5596689104266,-0.850035645395027));
#6574=CARTESIAN_POINT('Ctrl Pts',(94.6297924283201,1.55583523908449,-0.857032335277985));
#6575=CARTESIAN_POINT('Ctrl Pts',(94.6287649541035,1.5484605815015,-0.870278968726304));
#6576=CARTESIAN_POINT('Ctrl Pts',(94.6282806669416,1.54492867308116,-0.876533543389885));
#6577=CARTESIAN_POINT('Ctrl Pts',(94.6271159235648,1.53630071661163,-0.891598427471945));
#6578=CARTESIAN_POINT('Ctrl Pts',(94.6264378566784,1.53116661300014,-0.900386840922093));
#6579=CARTESIAN_POINT('Ctrl Pts',(94.6241488730038,1.51346745543387,-0.930094504792485));
#6580=CARTESIAN_POINT('Ctrl Pts',(94.6225587920112,1.500546390029,-0.950799768317442));
#6581=CARTESIAN_POINT('Ctrl Pts',(94.6109807819324,1.4021882411966,-1.10141077228003));
#6582=CARTESIAN_POINT('Ctrl Pts',(94.6017564364994,1.30044293397444,-1.21987593943647));
#6583=CARTESIAN_POINT('Ctrl Pts',(94.587963495248,1.13560490190286,-1.36739958152182));
#6584=CARTESIAN_POINT('Ctrl Pts',(94.5838025110408,1.08426244929982,-1.40845789016199));
#6585=CARTESIAN_POINT('Ctrl Pts',(94.5782210040343,1.01439392352613,-1.45824321403634));
#6586=CARTESIAN_POINT('Ctrl Pts',(94.5769030623765,0.997823487867752,-1.46963142879174));
#6587=CARTESIAN_POINT('Ctrl Pts',(94.5746984269852,0.970012038421088,-1.48805795181153));
#6588=CARTESIAN_POINT('Ctrl Pts',(94.5738178060399,0.958878854639757,-1.4952562150192));
#6589=CARTESIAN_POINT('Ctrl Pts',(94.5720818626744,0.93689257722526,-1.50912511848459));
#6590=CARTESIAN_POINT('Ctrl Pts',(94.5712269505008,0.926046222199189,-1.51580496904516));
#6591=CARTESIAN_POINT('Ctrl Pts',(94.5691478006734,0.899629571228397,-1.5316846102644));
#6592=CARTESIAN_POINT('Ctrl Pts',(94.56791928755,0.883989078416313,-1.54076421872661));
#6593=CARTESIAN_POINT('Ctrl Pts',(94.5636696552796,0.829797306962036,-1.57112683751982));
#6594=CARTESIAN_POINT('Ctrl Pts',(94.5606070933443,0.790597533044739,-1.59121276569145));
#6595=CARTESIAN_POINT('Ctrl Pts',(94.5487779965292,0.638703686695453,-1.66204423178195));
#6596=CARTESIAN_POINT('Ctrl Pts',(94.5397031430995,0.521579601218354,-1.70243379138357));
#6597=CARTESIAN_POINT('Ctrl Pts',(94.5256520476236,0.333967789323071,-1.74593742228245));
#6598=CARTESIAN_POINT('Ctrl Pts',(94.5206527168306,0.265843401143473,-1.7576009467397));
#6599=CARTESIAN_POINT('Ctrl Pts',(94.5145985063424,0.179954812375146,-1.76719599453683));
#6600=CARTESIAN_POINT('Ctrl Pts',(94.51339303078,0.162674405236508,-1.76887040560473));
#6601=CARTESIAN_POINT('Ctrl Pts',(94.5116051043233,0.136735611545647,-1.77100042786057));
#6602=CARTESIAN_POINT('Ctrl Pts',(94.5110130608204,0.12809447879119,-1.77164639682497));
#6603=CARTESIAN_POINT('Ctrl Pts',(94.5099449968422,0.112404824509095,-1.77270388391908));
#6604=CARTESIAN_POINT('Ctrl Pts',(94.5094678728085,0.105358286915062,-1.77313663876991));
#6605=CARTESIAN_POINT('Ctrl Pts',(94.50838327894,0.089255181541533,-1.77402925500626));
#6606=CARTESIAN_POINT('Ctrl Pts',(94.507777313679,0.0801974592629025,-1.77446179488423));
#6607=CARTESIAN_POINT('Ctrl Pts',(94.5059255905719,0.0523467292729324,-1.77557807713393));
#6608=CARTESIAN_POINT('Ctrl Pts',(94.5046916092063,0.0335451859166894,-1.77603279178416));
#6609=CARTESIAN_POINT('Ctrl Pts',(94.4959055546058,-0.101737711041205,-1.77715538839417));
#6610=CARTESIAN_POINT('Ctrl Pts',(94.4888337047168,-0.218042611905205,-1.76666248030984));
#6611=CARTESIAN_POINT('Ctrl Pts',(94.4772276850087,-0.403639267370296,-1.73129570381198));
#6612=CARTESIAN_POINT('Ctrl Pts',(94.4727598165035,-0.473884813714225,-1.71340059811568));
#6613=CARTESIAN_POINT('Ctrl Pts',(94.465292932081,-0.586319443726679,-1.67731302049721));
#6614=CARTESIAN_POINT('Ctrl Pts',(94.4623647378626,-0.629243204801126,-1.66168646304877));
#6615=CARTESIAN_POINT('Ctrl Pts',(94.4582165786619,-0.688041670339702,-1.63767561272757));
#6616=CARTESIAN_POINT('Ctrl Pts',(94.4570426939154,-0.70446547492639,-1.63067811324624));
#6617=CARTESIAN_POINT('Ctrl Pts',(94.455011021815,-0.732502024566366,-1.61823030589288));
#6618=CARTESIAN_POINT('Ctrl Pts',(94.4541573588965,-0.7441665278786,-1.61289947081182));
#6619=CARTESIAN_POINT('Ctrl Pts',(94.4525119703957,-0.766421460956895,-1.6024358607059));
#6620=CARTESIAN_POINT('Ctrl Pts',(94.4517209782419,-0.77702064512725,-1.59732321367596));
#6621=CARTESIAN_POINT('Ctrl Pts',(94.4496304809519,-0.804766808166873,-1.58359800028559));
#6622=CARTESIAN_POINT('Ctrl Pts',(94.4483249879578,-0.821825984324407,-1.57481244694178));
#6623=CARTESIAN_POINT('Ctrl Pts',(94.4434575053143,-0.88442219282675,-1.54128104622225));
#6624=CARTESIAN_POINT('Ctrl Pts',(94.4398360799854,-0.929008174541551,-1.51482433084457));
#6625=CARTESIAN_POINT('Ctrl Pts',(94.4271947209366,-1.07794586309346,-1.4173964114197));
#6626=CARTESIAN_POINT('Ctrl Pts',(94.4178878589543,-1.17585590146043,-1.33728696467246));
#6627=CARTESIAN_POINT('Ctrl Pts',(94.4056201385905,-1.29437266646587,-1.21716050776564));
#6628=CARTESIAN_POINT('Ctrl Pts',(94.4025450538604,-1.32320413351825,-1.18575358721403));
#6629=CARTESIAN_POINT('Ctrl Pts',(94.3976258957773,-1.36823721063815,-1.13300733898302));
#6630=CARTESIAN_POINT('Ctrl Pts',(94.3957509476169,-1.3851349601193,-1.11228594502442));
#6631=CARTESIAN_POINT('Ctrl Pts',(94.3931976575987,-1.40785265865109,-1.08310659393943));
#6632=CARTESIAN_POINT('Ctrl Pts',(94.3924946593182,-1.41407593190208,-1.07496896412983));
#6633=CARTESIAN_POINT('Ctrl Pts',(94.391306135188,-1.42454884714041,-1.06102610229231));
#6634=CARTESIAN_POINT('Ctrl Pts',(94.390818216899,-1.42883419686183,-1.05524814772104));
#6635=CARTESIAN_POINT('Ctrl Pts',(94.3897963916073,-1.43778092291671,-1.04303080777599));
#6636=CARTESIAN_POINT('Ctrl Pts',(94.389263009363,-1.44243433239643,-1.03658595938198));
#6637=CARTESIAN_POINT('Ctrl Pts',(94.3878058151533,-1.45509552981737,-1.01880017295125));
#6638=CARTESIAN_POINT('Ctrl Pts',(94.3868877959095,-1.46301406768841,-1.00739598004195));
#6639=CARTESIAN_POINT('Ctrl Pts',(94.3814164753894,-1.50979026480077,-0.938314368615776));
#6640=CARTESIAN_POINT('Ctrl Pts',(94.377047863597,-1.5453713826048,-0.878481684298969));
#6641=CARTESIAN_POINT('Ctrl Pts',(94.365808397107,-1.62880740975325,-0.717337255263666));
#6642=CARTESIAN_POINT('Ctrl Pts',(94.3590454624897,-1.67075320347701,-0.613327101261384));
#6643=CARTESIAN_POINT('Ctrl Pts',(94.3495897174998,-1.71375539714512,-0.468647005802481));
#6644=CARTESIAN_POINT('Ctrl Pts',(94.3471190248123,-1.72363898506094,-0.430878089029393));
#6645=CARTESIAN_POINT('Ctrl Pts',(94.3427032352319,-1.73884417224729,-0.363825095701174));
#6646=CARTESIAN_POINT('Ctrl Pts',(94.3407740140183,-1.74468912146665,-0.33467515565165));
#6647=CARTESIAN_POINT('Ctrl Pts',(94.337821830731,-1.75241740741335,-0.290394749305998));
#6648=CARTESIAN_POINT('Ctrl Pts',(94.336815974141,-1.75484213526017,-0.275363280772692));
#6649=CARTESIAN_POINT('Ctrl Pts',(94.3350537127347,-1.75872740736911,-0.249137263893315));
#6650=CARTESIAN_POINT('Ctrl Pts',(94.3343001116945,-1.76027504385336,-0.237956360619245));
#6651=CARTESIAN_POINT('Ctrl Pts',(94.3325884618629,-1.76353318301943,-0.212643813446523));
#6652=CARTESIAN_POINT('Ctrl Pts',(94.3316284728975,-1.76518056626541,-0.198504979566883));
#6653=CARTESIAN_POINT('Ctrl Pts',(94.3290252186059,-1.76916411776666,-0.160329551780577));
#6654=CARTESIAN_POINT('Ctrl Pts',(94.3273720755818,-1.77118023882369,-0.136263356070453));
#6655=CARTESIAN_POINT('Ctrl Pts',(94.3156374423573,-1.78190649835909,0.0332598718152109));
#6656=CARTESIAN_POINT('Ctrl Pts',(94.3050002933125,-1.77317629156353,0.179239185134527));
#6657=CARTESIAN_POINT('Ctrl Pts',(94.2887489612861,-1.73279864228695,0.39794817120223));
#6658=CARTESIAN_POINT('Ctrl Pts',(94.2831701989557,-1.71398765014958,0.47244305254472));
#6659=CARTESIAN_POINT('Ctrl Pts',(94.2765104011753,-1.68482978432634,0.562799568571997));
#6660=CARTESIAN_POINT('Ctrl Pts',(94.2752463043161,-1.67897938637629,0.580019862442365));
#6661=CARTESIAN_POINT('Ctrl Pts',(94.2733896120474,-1.66989862683795,0.605458924886001));
#6662=CARTESIAN_POINT('Ctrl Pts',(94.2727863537017,-1.66687000579552,0.613747770479729));
#6663=CARTESIAN_POINT('Ctrl Pts',(94.2717072831879,-1.66130891905485,0.628622715697216));
#6664=CARTESIAN_POINT('Ctrl Pts',(94.2712302331037,-1.65879886427694,0.635216636647327));
#6665=CARTESIAN_POINT('Ctrl Pts',(94.2701571770449,-1.65303607590358,0.650088368204042));
#6666=CARTESIAN_POINT('Ctrl Pts',(94.2695625324339,-1.64976039424339,0.658356897702939));
#6667=CARTESIAN_POINT('Ctrl Pts',(94.2677382642813,-1.6394617170447,0.683793378087505));
#6668=CARTESIAN_POINT('Ctrl Pts',(94.2665201854244,-1.63223156185939,0.700876808455042));
#6669=CARTESIAN_POINT('Ctrl Pts',(94.256608396622,-1.57060314459081,0.840363578805335));
#6670=CARTESIAN_POINT('Ctrl Pts',(94.2485557334798,-1.50277959030219,0.956383076887852));
#6671=CARTESIAN_POINT('Ctrl Pts',(94.2350372554962,-1.37142176960472,1.13205785874908));
#6672=CARTESIAN_POINT('Ctrl Pts',(94.2297162348126,-1.31543982584207,1.19664879509923));
#6673=CARTESIAN_POINT('Ctrl Pts',(94.2225401240605,-1.23674222722124,1.27522585634183));
#6674=CARTESIAN_POINT('Ctrl Pts',(94.2208564144403,-1.21805327461654,1.2930887171653));
#6675=CARTESIAN_POINT('Ctrl Pts',(94.2182040679773,-1.18831805343466,1.32029283383892));
#6676=CARTESIAN_POINT('Ctrl Pts',(94.2172475301206,-1.17753577151877,1.32991821147911));
#6677=CARTESIAN_POINT('Ctrl Pts',(94.2154522205512,-1.15719859193177,1.34763205839611));
#6678=CARTESIAN_POINT('Ctrl Pts',(94.2146148843366,-1.14767326845435,1.3557532227556));
#6679=CARTESIAN_POINT('Ctrl Pts',(94.2127295784184,-1.12614285228857,1.37372027078897));
#6680=CARTESIAN_POINT('Ctrl Pts',(94.2116794405166,-1.11409302617292,1.38351068244152));
#6681=CARTESIAN_POINT('Ctrl Pts',(94.2089639720216,-1.08279773853364,1.40826394574645));
#6682=CARTESIAN_POINT('Ctrl Pts',(94.2072895382155,-1.06337033869011,1.42299040885461));
#6683=CARTESIAN_POINT('Ctrl Pts',(94.1974899910886,-0.948971506818882,1.5060565745101));
#6684=CARTESIAN_POINT('Ctrl Pts',(94.1890276594979,-0.847751034353264,1.56526766842386));
#6685=CARTESIAN_POINT('Ctrl Pts',(94.175033136049,-0.673806282369953,1.64517257531713));
#6686=CARTESIAN_POINT('Ctrl Pts',(94.1695745905638,-0.604257828579552,1.67196923334007));
#6687=CARTESIAN_POINT('Ctrl Pts',(94.1623978404426,-0.508746285298949,1.70202823864681));
#6688=CARTESIAN_POINT('Ctrl Pts',(94.1605737214393,-0.48409674181734,1.70920255962396));
#6689=CARTESIAN_POINT('Ctrl Pts',(94.1574660661137,-0.441326924526078,1.7206512582471));
#6690=CARTESIAN_POINT('Ctrl Pts',(94.1561721174691,-0.423279337843018,1.72517966524375));
#6691=CARTESIAN_POINT('Ctrl Pts',(94.1542805455314,-0.396493761742497,1.73145489147676));
#6692=CARTESIAN_POINT('Ctrl Pts',(94.1536716955606,-0.387809074147365,1.7334207437585));
#6693=CARTESIAN_POINT('Ctrl Pts',(94.1525869896593,-0.372216694057411,1.7368271580589));
#6694=CARTESIAN_POINT('Ctrl Pts',(94.1521098294717,-0.365314815660281,1.73829195892311));
#6695=CARTESIAN_POINT('Ctrl Pts',(94.1510418766553,-0.349771159297787,1.74149415369455));
#6696=CARTESIAN_POINT('Ctrl Pts',(94.1504523796679,-0.34112498197185,1.74320839435481));
#6697=CARTESIAN_POINT('Ctrl Pts',(94.1486606026384,-0.314655763585711,1.74825185262594));
#6698=CARTESIAN_POINT('Ctrl Pts',(94.1474692822927,-0.296793587058729,1.75137272416074));
#6699=CARTESIAN_POINT('Ctrl Pts',(94.1402507099039,-0.18719141575427,1.76879728195943));
#6700=CARTESIAN_POINT('Ctrl Pts',(94.1345305521696,-0.0944832916806178,
1.77616485190593));
#6701=CARTESIAN_POINT('Ctrl Pts',(94.1211072459206,0.124062194002053,1.7763635018049));
#6702=CARTESIAN_POINT('Ctrl Pts',(94.1134354308902,0.249382072983139,1.76314017233794));
#6703=CARTESIAN_POINT('Ctrl Pts',(94.1037857514685,0.395758592039518,1.7317670536397));
#6704=CARTESIAN_POINT('Ctrl Pts',(94.102222699047,0.419159227200112,1.7262524279553));
#6705=CARTESIAN_POINT('Ctrl Pts',(94.0996319497146,0.457381321142991,1.71642197715427));
#6706=CARTESIAN_POINT('Ctrl Pts',(94.0986131679651,0.472271655514866,1.71238475083716));
#6707=CARTESIAN_POINT('Ctrl Pts',(94.0967567477616,0.499138899895942,1.70472313198146));
#6708=CARTESIAN_POINT('Ctrl Pts',(94.0959213179238,0.511133810466153,1.70116513370024));
#6709=CARTESIAN_POINT('Ctrl Pts',(94.0941067450424,0.536973714200472,1.6932023973668));
#6710=CARTESIAN_POINT('Ctrl Pts',(94.0931262177289,0.550804168837922,1.68875394119343));
#6711=CARTESIAN_POINT('Ctrl Pts',(94.0903605171287,0.589434477825859,1.67580378598754));
#6712=CARTESIAN_POINT('Ctrl Pts',(94.0885629837096,0.614102057187853,1.66692227421533));
#6713=CARTESIAN_POINT('Ctrl Pts',(94.08064705375,0.720779724255802,1.62582395349118));
#6714=CARTESIAN_POINT('Ctrl Pts',(94.0743500233791,0.800514041173156,1.5880806627173));
#6715=CARTESIAN_POINT('Ctrl Pts',(94.0636341060031,0.928736585387347,1.51526802133098));
#6716=CARTESIAN_POINT('Ctrl Pts',(94.0592811121909,0.978860053808308,1.48338180427142));
#6717=CARTESIAN_POINT('Ctrl Pts',(94.049209552882,1.09138927152295,1.40360499193183));
#6718=CARTESIAN_POINT('Ctrl Pts',(94.0435138787308,1.15240853706415,1.3539552333509));
#6719=CARTESIAN_POINT('Ctrl Pts',(94.0370631143474,1.2202189990265,1.29086273863887));
#6720=CARTESIAN_POINT('Ctrl Pts',(94.0360931201038,1.23038027722571,1.28118125961192));
#6721=CARTESIAN_POINT('Ctrl Pts',(94.0345849706424,1.24613892918658,1.26580627822359));
#6722=CARTESIAN_POINT('Ctrl Pts',(94.0340410286497,1.25181423795601,1.26019398696335));
#6723=CARTESIAN_POINT('Ctrl Pts',(94.0330133879427,1.26252392649933,1.24945947219386));
#6724=CARTESIAN_POINT('Ctrl Pts',(94.032529179365,1.26756529886373,1.24434474824296));
#6725=CARTESIAN_POINT('Ctrl Pts',(94.0313650360795,1.27967052803989,1.23191348153976));
#6726=CARTESIAN_POINT('Ctrl Pts',(94.0306874842556,1.28670295459727,1.22456645604751));
#6727=CARTESIAN_POINT('Ctrl Pts',(94.0282786440752,1.31163905321841,1.19806282812318));
#6728=CARTESIAN_POINT('Ctrl Pts',(94.0265721063015,1.32918211883409,1.17856973272622));
#6729=CARTESIAN_POINT('Ctrl Pts',(94.0222259608199,1.37331018923433,1.12729727115831));
#6730=CARTESIAN_POINT('Ctrl Pts',(94.0196201925805,1.39922737645146,1.09496264935401));
#6731=CARTESIAN_POINT('Ctrl Pts',(94.0121665066269,1.47082950822803,0.99893166328431));
#6732=CARTESIAN_POINT('Ctrl Pts',(94.0073958457916,1.51346045508009,0.93308201223802));
#6733=CARTESIAN_POINT('Ctrl Pts',(93.9967111760042,1.59791977048567,0.781517385489466));
#6734=CARTESIAN_POINT('Ctrl Pts',(93.9907839085201,1.63747641358145,0.694827125005744));
#6735=CARTESIAN_POINT('Ctrl Pts',(93.9831734663719,1.67747553060869,0.584494698040664));
#6736=CARTESIAN_POINT('Ctrl Pts',(93.9817200599898,1.684658625819,0.563456697769412));
#6737=CARTESIAN_POINT('Ctrl Pts',(93.9793500497264,1.69562690680731,0.529245785857968));
#6738=CARTESIAN_POINT('Ctrl Pts',(93.9784415591389,1.69965789995779,0.516153769966571));
#6739=CARTESIAN_POINT('Ctrl Pts',(93.9766834126647,1.70712392480102,0.490869026476544));
#6740=CARTESIAN_POINT('Ctrl Pts',(93.9758345308789,1.71058075560855,0.478683569731445));
#6741=CARTESIAN_POINT('Ctrl Pts',(93.9738450847763,1.71833685726729,0.45018559306448));
#6742=CARTESIAN_POINT('Ctrl Pts',(93.9727013100048,1.72253458634699,0.433846963532261));
#6743=CARTESIAN_POINT('Ctrl Pts',(93.9688837436778,1.73567971159305,0.379481262805467));
#6744=CARTESIAN_POINT('Ctrl Pts',(93.966177910031,1.74360480179457,0.341221293699562));
#6745=CARTESIAN_POINT('Ctrl Pts',(93.9594249809633,1.75999662247539,0.246451595404281));
#6746=CARTESIAN_POINT('Ctrl Pts',(93.9553391945997,1.76701020958113,0.189737654203443));
#6747=CARTESIAN_POINT('Ctrl Pts',(93.9483782134909,1.77419824065539,0.0938560027675912));
#6748=CARTESIAN_POINT('Ctrl Pts',(93.9455312101927,1.7758324567088,0.054838590856963));
#6749=CARTESIAN_POINT('Ctrl Pts',(93.9411336659243,1.77636761854763,-0.00532194227614969));
#6750=CARTESIAN_POINT('Ctrl Pts',(93.9395886383419,1.77617867042149,-0.0264394646778253));
#6751=CARTESIAN_POINT('Ctrl Pts',(93.938045236354,1.77561363622783,-0.0475423741708462));
#6752=CARTESIAN_POINT('',(93.9795659395437,0.000115947507982164,1.77624999621567));
#6753=CARTESIAN_POINT('Ctrl Pts',(93.7915308013958,1.77561364010973,-0.0475422291890938));
#6754=CARTESIAN_POINT('Ctrl Pts',(93.7928573604259,1.77610450162403,-0.0292094666102127));
#6755=CARTESIAN_POINT('Ctrl Pts',(93.7941784581398,1.77631154895408,-0.0108651108999133));
#6756=CARTESIAN_POINT('Ctrl Pts',(93.7980361553455,1.77608444226741,0.0430336293841766));
#6757=CARTESIAN_POINT('Ctrl Pts',(93.8005493957931,1.77486745046972,0.0785733486572298));
#6758=CARTESIAN_POINT('Ctrl Pts',(93.8038236861351,1.77183360385389,0.125723749035798));
#6759=CARTESIAN_POINT('Ctrl Pts',(93.8046285780797,1.77096757914434,0.137384980726422));
#6760=CARTESIAN_POINT('Ctrl Pts',(93.8058874411011,1.76942135888394,0.155748107009445));
#6761=CARTESIAN_POINT('Ctrl Pts',(93.8063454709787,1.76881810978186,0.162455890798343));
#6762=CARTESIAN_POINT('Ctrl Pts',(93.8072973684724,1.76747881301121,0.176455123791574));
#6763=CARTESIAN_POINT('Ctrl Pts',(93.8077907979097,1.76673577018263,0.183745710675326));
#6764=CARTESIAN_POINT('Ctrl Pts',(93.8090176475938,1.7647663778025,0.201951305055927));
#6765=CARTESIAN_POINT('Ctrl Pts',(93.8097480090473,1.76348384235142,0.212860167457891));
#6766=CARTESIAN_POINT('Ctrl Pts',(93.812610738017,1.75802323951052,0.25586279455385));
#6767=CARTESIAN_POINT('Ctrl Pts',(93.8147044347149,1.75306930253835,0.287853799522207));
#6768=CARTESIAN_POINT('Ctrl Pts',(93.8204090383504,1.73696583841422,0.375865112932617));
#6769=CARTESIAN_POINT('Ctrl Pts',(93.8239538103413,1.72398465243174,0.431512135220726));
#6770=CARTESIAN_POINT('Ctrl Pts',(93.8364607367806,1.66840000086416,0.62672147590001));
#6771=CARTESIAN_POINT('Ctrl Pts',(93.8452834387934,1.61133507624045,0.761533810506193));
#6772=CARTESIAN_POINT('Ctrl Pts',(93.8562719304892,1.52637631443935,0.908747203367535));
#6773=CARTESIAN_POINT('Ctrl Pts',(93.857845444609,1.51389298538698,0.929394464576138));
#6774=CARTESIAN_POINT('Ctrl Pts',(93.8603712013899,1.49338508334739,0.961804304282125));
#6775=CARTESIAN_POINT('Ctrl Pts',(93.8613134316003,1.48563266934305,0.973736144355019));
#6776=CARTESIAN_POINT('Ctrl Pts',(93.8630127762464,1.47147483562486,0.994963960133127));
#6777=CARTESIAN_POINT('Ctrl Pts',(93.8637678611087,1.46512249966352,1.00429454079167));
#6778=CARTESIAN_POINT('Ctrl Pts',(93.8655498658519,1.44999036387896,1.02607212574692));
#6779=CARTESIAN_POINT('Ctrl Pts',(93.8665794986688,1.44113865174967,1.03846782509942));
#6780=CARTESIAN_POINT('Ctrl Pts',(93.8696391498019,1.41452427399495,1.07474219791824));
#6781=CARTESIAN_POINT('Ctrl Pts',(93.8716861089007,1.39632044878063,1.09828900201252));
#6782=CARTESIAN_POINT('Ctrl Pts',(93.8764736987312,1.35285618195068,1.15168238188039));
#6783=CARTESIAN_POINT('Ctrl Pts',(93.8792293519519,1.32718531840914,1.1811735293513));
#6784=CARTESIAN_POINT('Ctrl Pts',(93.8900232902046,1.22408627105126,1.29200820653384));
#6785=CARTESIAN_POINT('Ctrl Pts',(93.8982868212188,1.13998935857522,1.36678178112968));
#6786=CARTESIAN_POINT('Ctrl Pts',(93.9114994856624,0.993669003969397,1.47392637938748));
#6787=CARTESIAN_POINT('Ctrl Pts',(93.9164843357838,0.935588284761137,1.51146077610724));
#6788=CARTESIAN_POINT('Ctrl Pts',(93.922260891919,0.863396848085454,1.55235377511014));
#6789=CARTESIAN_POINT('Ctrl Pts',(93.9232191022768,0.851250909193058,1.55904723466866));
#6790=CARTESIAN_POINT('Ctrl Pts',(93.9247131027331,0.83202422117582,1.5693511039708));
#6791=CARTESIAN_POINT('Ctrl Pts',(93.9252545100866,0.824995802865499,1.57305725376944));
#6792=CARTESIAN_POINT('Ctrl Pts',(93.926280454821,0.811556197828013,1.58002922829377));
#6793=CARTESIAN_POINT('Ctrl Pts',(93.9267654682168,0.805149753671243,1.58330341387512));
#6794=CARTESIAN_POINT('Ctrl Pts',(93.9279357653475,0.789567228979204,1.59114824537304));
#6795=CARTESIAN_POINT('Ctrl Pts',(93.9286185998461,0.780370972218809,1.5956786349831));
#6796=CARTESIAN_POINT('Ctrl Pts',(93.9310695456324,0.747007764903059,1.61175706163288));
#6797=CARTESIAN_POINT('Ctrl Pts',(93.9328117523522,0.722618314996183,1.62283837202576));
#6798=CARTESIAN_POINT('Ctrl Pts',(93.937275144223,0.658686546528779,1.65015834980396));
#6799=CARTESIAN_POINT('Ctrl Pts',(93.9399601517045,0.618791118764905,1.6655295168743));
#6800=CARTESIAN_POINT('Ctrl Pts',(93.9514338938808,0.444256618011175,1.72563669884012));
#6801=CARTESIAN_POINT('Ctrl Pts',(93.9599404123782,0.30509109801814,1.75559272208157));
#6802=CARTESIAN_POINT('Ctrl Pts',(93.9712136706598,0.128318363072791,1.77196819027313));
#6803=CARTESIAN_POINT('Ctrl Pts',(93.9735051847306,0.0927049881957018,1.77418781121198));
#6804=CARTESIAN_POINT('Ctrl Pts',(93.9765702297719,0.0456782895515519,1.77569902331361));
#6805=CARTESIAN_POINT('Ctrl Pts',(93.9773146368292,0.0343028600437258,1.7759551885171));
#6806=CARTESIAN_POINT('Ctrl Pts',(93.9785620793822,0.0153229027538503,1.7762001822216));
#6807=CARTESIAN_POINT('Ctrl Pts',(93.9790632566766,0.00771940838996888,
1.77624949988782));
#6808=CARTESIAN_POINT('Ctrl Pts',(93.9795659395437,0.000115947507982164,
1.77624999621567));
#6809=CARTESIAN_POINT('Ctrl Pts',(93.9795659773891,0.000115375067715305,
1.77624999625295));
#6810=CARTESIAN_POINT('Ctrl Pts',(93.9799864663399,-0.00624483932767286,
1.77625040937619));
#6811=CARTESIAN_POINT('Ctrl Pts',(93.9804080037495,-0.0126049561014548,
1.77621666149281));
#6812=CARTESIAN_POINT('Ctrl Pts',(93.9813988129797,-0.0275156646565273,
1.77605745346026));
#6813=CARTESIAN_POINT('Ctrl Pts',(93.9819689297411,-0.0360657251495172,
1.77590440307868));
#6814=CARTESIAN_POINT('Ctrl Pts',(93.98343137621,-0.0579197181264248,1.77535532127359));
#6815=CARTESIAN_POINT('Ctrl Pts',(93.9843264205943,-0.0712207125656861,
1.77487148939002));
#6816=CARTESIAN_POINT('Ctrl Pts',(93.9865529071123,-0.104117071083033,1.77330449236378));
#6817=CARTESIAN_POINT('Ctrl Pts',(93.9878897449017,-0.123701896461083,1.77204598528339));
#6818=CARTESIAN_POINT('Ctrl Pts',(93.9933456945305,-0.2029310194927,1.76563497522455));
#6819=CARTESIAN_POINT('Ctrl Pts',(93.9975467803286,-0.262312007469336,1.7577937473307));
#6820=CARTESIAN_POINT('Ctrl Pts',(94.0054540066584,-0.371190145239888,1.73777663948774));
#6821=CARTESIAN_POINT('Ctrl Pts',(94.0091355111197,-0.420781041899192,1.72643926139459));
#6822=CARTESIAN_POINT('Ctrl Pts',(94.0178024421711,-0.535457364390115,1.69498748429302));
#6823=CARTESIAN_POINT('Ctrl Pts',(94.0228014371669,-0.600010798160375,1.67322569972188));
#6824=CARTESIAN_POINT('Ctrl Pts',(94.0321368688422,-0.719254663214412,1.62523645610704));
#6825=CARTESIAN_POINT('Ctrl Pts',(94.0364784444672,-0.774169849893795,1.59980729644811));
#6826=CARTESIAN_POINT('Ctrl Pts',(94.0416052622191,-0.839404867044646,1.56545167934388));
#6827=CARTESIAN_POINT('Ctrl Pts',(94.0425195532581,-0.85105502554311,1.55914876165928));
#6828=CARTESIAN_POINT('Ctrl Pts',(94.0439607772313,-0.86946219420347,1.54892238990078));
#6829=CARTESIAN_POINT('Ctrl Pts',(94.0444927125386,-0.876265440262095,1.54508380394872));
#6830=CARTESIAN_POINT('Ctrl Pts',(94.0455073951989,-0.889265132637704,1.53763552431227));
#6831=CARTESIAN_POINT('Ctrl Pts',(94.045990545695,-0.895465337666658,1.53403302203291));
#6832=CARTESIAN_POINT('Ctrl Pts',(94.0470646539551,-0.909267801341845,1.52590118690606));
#6833=CARTESIAN_POINT('Ctrl Pts',(94.0476543797019,-0.916858479024284,1.52135232747974));
#6834=CARTESIAN_POINT('Ctrl Pts',(94.0496987468193,-0.943201959374167,1.50529670814512));
#6835=CARTESIAN_POINT('Ctrl Pts',(94.0511360833147,-0.961775557561119,1.4934979071862));
#6836=CARTESIAN_POINT('Ctrl Pts',(94.0608948230114,-1.08779375687798,1.41011910048729));
#6837=CARTESIAN_POINT('Ctrl Pts',(94.068663302468,-1.18738682820815,1.32734764794752));
#6838=CARTESIAN_POINT('Ctrl Pts',(94.0818336518972,-1.3358705542575,1.173736001161));
#6839=CARTESIAN_POINT('Ctrl Pts',(94.0871037402546,-1.39018901868765,1.10886360070515));
#6840=CARTESIAN_POINT('Ctrl Pts',(94.0942177698618,-1.45475314108468,1.01951927736893));
#6841=CARTESIAN_POINT('Ctrl Pts',(94.0958940188898,-1.46936975471025,0.998337955199077));
#6842=CARTESIAN_POINT('Ctrl Pts',(94.0985372043243,-1.49145570736709,0.964796418837553));
#6843=CARTESIAN_POINT('Ctrl Pts',(94.0994921812177,-1.49924355441912,0.952649463705689));
#6844=CARTESIAN_POINT('Ctrl Pts',(94.1012860649156,-1.51351036467539,0.929788773823545));
#6845=CARTESIAN_POINT('Ctrl Pts',(94.102123556014,-1.52002574889904,0.919098741559542));
#6846=CARTESIAN_POINT('Ctrl Pts',(94.1040112050055,-1.53438316400193,0.894971730459357));
#6847=CARTESIAN_POINT('Ctrl Pts',(94.1050635558847,-1.54216266457929,0.881498940082484));
#6848=CARTESIAN_POINT('Ctrl Pts',(94.107788904356,-1.56172906747557,0.846561279386078));
#6849=CARTESIAN_POINT('Ctrl Pts',(94.1094711183245,-1.5732505281921,0.82495233290072));
#6850=CARTESIAN_POINT('Ctrl Pts',(94.1189551939107,-1.63510497615374,0.702930518248901));
#6851=CARTESIAN_POINT('Ctrl Pts',(94.1270649341482,-1.67626391742539,0.598173178856525));
#6852=CARTESIAN_POINT('Ctrl Pts',(94.1409556276356,-1.72872753119102,0.415473076769958));
#6853=CARTESIAN_POINT('Ctrl Pts',(94.1466655916062,-1.74526506333845,0.339363410515984));
#6854=CARTESIAN_POINT('Ctrl Pts',(94.154131582678,-1.76064256187031,0.236416361928378));
#6855=CARTESIAN_POINT('Ctrl Pts',(94.156000806987,-1.76394835736683,0.210336076608996));
#6856=CARTESIAN_POINT('Ctrl Pts',(94.1591765177528,-1.76863780204441,0.165357040272354));
#6857=CARTESIAN_POINT('Ctrl Pts',(94.1604939932711,-1.77030018113251,0.146492204976438));
#6858=CARTESIAN_POINT('Ctrl Pts',(94.1624129760162,-1.77230472580304,0.118660887134308));
#6859=CARTESIAN_POINT('Ctrl Pts',(94.163026163234,-1.77288111461821,0.109713305489057));
#6860=CARTESIAN_POINT('Ctrl Pts',(94.1641152832622,-1.77379002903949,0.0937165263173397));
#6861=CARTESIAN_POINT('Ctrl Pts',(94.1645925717111,-1.77414832911114,0.0866692890639678));
#6862=CARTESIAN_POINT('Ctrl Pts',(94.1656567692218,-1.77485708536297,0.0708734117247586));
#6863=CARTESIAN_POINT('Ctrl Pts',(94.1662424317102,-1.77518486814393,0.0621241173604022));
#6864=CARTESIAN_POINT('Ctrl Pts',(94.1680103058163,-1.77598353932047,0.0355561584982368));
#6865=CARTESIAN_POINT('Ctrl Pts',(94.1691819780722,-1.77625094277533,0.0177318981764129));
#6866=CARTESIAN_POINT('Ctrl Pts',(94.1767779208922,-1.77624475354874,-0.0989854299933978));
#6867=CARTESIAN_POINT('Ctrl Pts',(94.1828502268093,-1.76798094835211,-0.197716617637565));
#6868=CARTESIAN_POINT('Ctrl Pts',(94.1965998990649,-1.73075146818123,-0.418571406489691));
#6869=CARTESIAN_POINT('Ctrl Pts',(94.2042570865877,-1.69700328735534,-0.539330991453883));
#6870=CARTESIAN_POINT('Ctrl Pts',(94.2138923540971,-1.64203770939722,-0.677751697054265));
#6871=CARTESIAN_POINT('Ctrl Pts',(94.2154520239907,-1.63277075284724,-0.699781953129171));
#6872=CARTESIAN_POINT('Ctrl Pts',(94.2179522869917,-1.61735525944735,-0.734454479384979));
#6873=CARTESIAN_POINT('Ctrl Pts',(94.2188830107744,-1.61149606112767,-0.747222753522626));
#6874=CARTESIAN_POINT('Ctrl Pts',(94.2206566495629,-1.60010728451435,-0.77128387329668));
#6875=CARTESIAN_POINT('Ctrl Pts',(94.2214984711711,-1.59460802119548,-0.78259017362021));
#6876=CARTESIAN_POINT('Ctrl Pts',(94.2234312522828,-1.58177197788939,-0.808283531765959));
#6877=CARTESIAN_POINT('Ctrl Pts',(94.2245248616109,-1.5743581755155,-0.822630635731021));
#6878=CARTESIAN_POINT('Ctrl Pts',(94.2274354808607,-1.55423614550455,-0.860301994549673));
#6879=CARTESIAN_POINT('Ctrl Pts',(94.2292639374394,-1.5411990215746,-0.883444939763982));
#6880=CARTESIAN_POINT('Ctrl Pts',(94.2429048972358,-1.4410785883627,-1.05220938852991));
#6881=CARTESIAN_POINT('Ctrl Pts',(94.255477346546,-1.33405470352637,-1.1849591379934));
#6882=CARTESIAN_POINT('Ctrl Pts',(94.2716191486411,-1.17080256151959,-1.33683724113822));
#6883=CARTESIAN_POINT('Ctrl Pts',(94.2754351091337,-1.13010476343109,-1.37141416390176));
#6884=CARTESIAN_POINT('Ctrl Pts',(94.2800361410189,-1.07775614595733,-1.4119740331767));
#6885=CARTESIAN_POINT('Ctrl Pts',(94.2809220133478,-1.0675192599132,-1.41972942293127));
#6886=CARTESIAN_POINT('Ctrl Pts',(94.2823290258082,-1.05099206811049,-1.43197045773407));
#6887=CARTESIAN_POINT('Ctrl Pts',(94.2828547849573,-1.04475527278908,-1.43652711244484));
#6888=CARTESIAN_POINT('Ctrl Pts',(94.2838662854216,-1.03263391462063,-1.44526237872308));
#6889=CARTESIAN_POINT('Ctrl Pts',(94.2843523422996,-1.02675332044446,-1.4494460204602));
#6890=CARTESIAN_POINT('Ctrl Pts',(94.2854415199169,-1.01345385765933,-1.45878612710112));
#6891=CARTESIAN_POINT('Ctrl Pts',(94.2860432880951,-1.00602070449744,-1.46392214170211));
#6892=CARTESIAN_POINT('Ctrl Pts',(94.288174498974,-0.97940562305954,-1.48201364950666));
#6893=CARTESIAN_POINT('Ctrl Pts',(94.2896846547853,-0.960009133399487,-1.4946512696149));
#6894=CARTESIAN_POINT('Ctrl Pts',(94.2994140133874,-0.831983168734802,-1.57454458702625));
#6895=CARTESIAN_POINT('Ctrl Pts',(94.307103738188,-0.716602985685367,-1.63029889325728));
#6896=CARTESIAN_POINT('Ctrl Pts',(94.3201771133632,-0.516852715869432,-1.70147808438705));
#6897=CARTESIAN_POINT('Ctrl Pts',(94.3254324990652,-0.435574582192307,-1.72407565167617));
#6898=CARTESIAN_POINT('Ctrl Pts',(94.3325286132007,-0.32781886934016,-1.74592648756649));
#6899=CARTESIAN_POINT('Ctrl Pts',(94.3342027055609,-0.302525532545672,-1.75048641927848));
#6900=CARTESIAN_POINT('Ctrl Pts',(94.3368432488757,-0.262897848178668,-1.75674607638215));
#6901=CARTESIAN_POINT('Ctrl Pts',(94.3377977805717,-0.248626005484601,-1.7588226585455));
#6902=CARTESIAN_POINT('Ctrl Pts',(94.3395912693935,-0.221920577800965,-1.76237682160551));
#6903=CARTESIAN_POINT('Ctrl Pts',(94.3404288165683,-0.209493518106686,-1.76389717846503));
#6904=CARTESIAN_POINT('Ctrl Pts',(94.3423171787955,-0.181580944289874,-1.76701294550767));
#6905=CARTESIAN_POINT('Ctrl Pts',(94.3433701941917,-0.166088607430766,-1.76853638256265));
#6906=CARTESIAN_POINT('Ctrl Pts',(94.3460984909525,-0.12614695295972,-1.77193460327382));
#6907=CARTESIAN_POINT('Ctrl Pts',(94.3477830224392,-0.101675936882023,-1.77350703171133));
#6908=CARTESIAN_POINT('Ctrl Pts',(94.3570688884535,0.0321363423118928,-1.77932691128762));
#6909=CARTESIAN_POINT('Ctrl Pts',(94.3649607784222,0.1416419557808,-1.77396938100256));
#6910=CARTESIAN_POINT('Ctrl Pts',(94.3787911940914,0.329085510764859,-1.74732855232778));
#6911=CARTESIAN_POINT('Ctrl Pts',(94.3846621399857,0.407382231093236,-1.7307498218207));
#6912=CARTESIAN_POINT('Ctrl Pts',(94.3923123967429,0.509953960203574,-1.70168213987478));
#6913=CARTESIAN_POINT('Ctrl Pts',(94.394209585663,0.535444238820346,-1.69383433808562));
#6914=CARTESIAN_POINT('Ctrl Pts',(94.3974273775047,0.578909960521693,-1.67937298799806));
#6915=CARTESIAN_POINT('Ctrl Pts',(94.3987593336871,0.596972593103999,-1.67303740912064));
#6916=CARTESIAN_POINT('Ctrl Pts',(94.4006951674767,0.62337693245032,-1.66329381825862));
#6917=CARTESIAN_POINT('Ctrl Pts',(94.4013110078691,0.631800100755204,-1.66011257669175));
#6918=CARTESIAN_POINT('Ctrl Pts',(94.4024028632148,0.646781927089882,-1.65432373099171));
#6919=CARTESIAN_POINT('Ctrl Pts',(94.402880265026,0.653349647123499,-1.65174093362369));
#6920=CARTESIAN_POINT('Ctrl Pts',(94.4039423113655,0.667998671628792,-1.64587906207647));
#6921=CARTESIAN_POINT('Ctrl Pts',(94.4045257381725,0.676071406820056,-1.64257954850405));
#6922=CARTESIAN_POINT('Ctrl Pts',(94.4062797246879,0.700404904422821,-1.63242409693122));
#6923=CARTESIAN_POINT('Ctrl Pts',(94.4074399857254,0.716588657862136,-1.62538494386275));
#6924=CARTESIAN_POINT('Ctrl Pts',(94.4152914120526,0.826455729855655,-1.57563798835702));
#6925=CARTESIAN_POINT('Ctrl Pts',(94.4215989434173,0.916388648129644,-1.52509064329707));
#6926=CARTESIAN_POINT('Ctrl Pts',(94.4330105864461,1.06993965989721,-1.42027149192713));
#6927=CARTESIAN_POINT('Ctrl Pts',(94.4380953728761,1.13507386099655,-1.36877615768248));
#6928=CARTESIAN_POINT('Ctrl Pts',(94.4464479671082,1.2330181228705,-1.27952677679979));
#6929=CARTESIAN_POINT('Ctrl Pts',(94.4496191159074,1.26824979647491,-1.24461409073309));
#6930=CARTESIAN_POINT('Ctrl Pts',(94.4540527565757,1.31447050987135,-1.19480914062528));
#6931=CARTESIAN_POINT('Ctrl Pts',(94.4552599246653,1.32675798727047,-1.18114978113743));
#6932=CARTESIAN_POINT('Ctrl Pts',(94.457331060941,1.34732043012408,-1.15756580730417));
#6933=CARTESIAN_POINT('Ctrl Pts',(94.4581904725254,1.35570317701682,-1.14773682542959));
#6934=CARTESIAN_POINT('Ctrl Pts',(94.4598346093449,1.37145199675288,-1.12885766402803));
#6935=CARTESIAN_POINT('Ctrl Pts',(94.4606184760101,1.3788375838117,-1.11982458948292));
#6936=CARTESIAN_POINT('Ctrl Pts',(94.4624620199673,1.39591755225327,-1.09850947408002));
#6937=CARTESIAN_POINT('Ctrl Pts',(94.4635245125744,1.40553956938392,-1.08617096666951));
#6938=CARTESIAN_POINT('Ctrl Pts',(94.4672702895434,1.43868045069771,-1.0424958885603));
#6939=CARTESIAN_POINT('Ctrl Pts',(94.4699868438229,1.46132293428499,-1.01051174273858));
#6940=CARTESIAN_POINT('Ctrl Pts',(94.4817551455758,1.5535018962888,-0.870718259878636));
#6941=CARTESIAN_POINT('Ctrl Pts',(94.4911663835455,1.61229931143434,-0.756307146531691));
#6942=CARTESIAN_POINT('Ctrl Pts',(94.5056833479908,1.68358186870427,-0.570621332588836));
#6943=CARTESIAN_POINT('Ctrl Pts',(94.5108035080017,1.70494874963744,-0.503198064602601));
#6944=CARTESIAN_POINT('Ctrl Pts',(94.5169846278853,1.72653493725547,-0.41767062453911));
#6945=CARTESIAN_POINT('Ctrl Pts',(94.5182027613506,1.73057485073023,-0.400602526405938));
#6946=CARTESIAN_POINT('Ctrl Pts',(94.5200055535634,1.73623963466528,-0.374982233421327));
#6947=CARTESIAN_POINT('Ctrl Pts',(94.5206000320464,1.73805540695714,-0.366473948232745));
#6948=CARTESIAN_POINT('Ctrl Pts',(94.5216225307759,1.74108889726297,-0.35172983136979));
#6949=CARTESIAN_POINT('Ctrl Pts',(94.522052145146,1.74233574687794,-0.345500464503926));
#6950=CARTESIAN_POINT('Ctrl Pts',(94.5230625809734,1.74520244171498,-0.33076792472615));
#6951=CARTESIAN_POINT('Ctrl Pts',(94.5236417864844,1.74679358884587,-0.322259442687384));
#6952=CARTESIAN_POINT('Ctrl Pts',(94.5253697244878,1.75138057275906,-0.296698336754262));
#6953=CARTESIAN_POINT('Ctrl Pts',(94.5265086023851,1.75418945361529,-0.279612641735894));
#6954=CARTESIAN_POINT('Ctrl Pts',(94.5323275997515,1.76739053090824,-0.191262000545466));
#6955=CARTESIAN_POINT('Ctrl Pts',(94.5368220546751,1.77368748547977,-0.119480554701164));
#6956=CARTESIAN_POINT('Ctrl Pts',(94.5412649413994,1.77561364082571,-0.0475422024484629));
#6957=CARTESIAN_POINT('Origin',(88.3562164250559,0.,0.));
#6958=CARTESIAN_POINT('',(95.4381488292622,1.77561363320029,-0.0475424872431835));
#6959=CARTESIAN_POINT('',(95.2889037169497,1.77561363837295,-0.0475422940546111));
#6960=CARTESIAN_POINT('',(88.3562164250559,1.77561363837197,-0.0475422940912398));
#6961=CARTESIAN_POINT('',(94.877703379636,0.000780936357206753,1.77624982832889));
#6962=CARTESIAN_POINT('Ctrl Pts',(95.4381488292622,1.77561363320029,-0.0475424872432087));
#6963=CARTESIAN_POINT('Ctrl Pts',(95.4324265684948,1.77311855787188,-0.14072839370037));
#6964=CARTESIAN_POINT('Ctrl Pts',(95.4267129126685,1.76329062656178,-0.23361968687051));
#6965=CARTESIAN_POINT('Ctrl Pts',(95.4181001991702,1.73839047815768,-0.367259235214042));
#6966=CARTESIAN_POINT('Ctrl Pts',(95.415363519225,1.72907800086031,-0.408863812839485));
#6967=CARTESIAN_POINT('Ctrl Pts',(95.4114150747514,1.71375977071512,-0.467343100896787));
#6968=CARTESIAN_POINT('Ctrl Pts',(95.4102423138545,1.70898123014907,-0.48452579138951));
#6969=CARTESIAN_POINT('Ctrl Pts',(95.4082203867911,1.70035980048995,-0.513811021492881));
#6970=CARTESIAN_POINT('Ctrl Pts',(95.4073754145735,1.69664431831655,-0.525949864298036));
#6971=CARTESIAN_POINT('Ctrl Pts',(95.4056345502037,1.68876217890978,-0.550748561096265));
#6972=CARTESIAN_POINT('Ctrl Pts',(95.4047382763972,1.68458251974351,-0.563403400592129));
#6973=CARTESIAN_POINT('Ctrl Pts',(95.4024548818364,1.67363046476664,-0.595351317138518));
#6974=CARTESIAN_POINT('Ctrl Pts',(95.4010615152036,1.66666676205364,-0.614576249658972));
#6975=CARTESIAN_POINT('Ctrl Pts',(95.3948711223093,1.63451435575078,-0.698772012019242));
#6976=CARTESIAN_POINT('Ctrl Pts',(95.3899601326701,1.60584997808338,-0.762340582429073));
#6977=CARTESIAN_POINT('Ctrl Pts',(95.379491207287,1.53822869151577,-0.891463177412685));
#6978=CARTESIAN_POINT('Ctrl Pts',(95.3739253392272,1.49863404050213,-0.95652957657421));
#6979=CARTESIAN_POINT('Ctrl Pts',(95.3621965732459,1.406629878176,-1.08791791780787));
#6980=CARTESIAN_POINT('Ctrl Pts',(95.3560482676687,1.35340640349611,-1.153458606964));
#6981=CARTESIAN_POINT('Ctrl Pts',(95.3488597086622,1.28330396284671,-1.22822012633944));
#6982=CARTESIAN_POINT('Ctrl Pts',(95.3475975998636,1.27068138661002,-1.24127459387855));
#6983=CARTESIAN_POINT('Ctrl Pts',(95.3457432337999,1.25163345025343,-1.26037912773783));
#6984=CARTESIAN_POINT('Ctrl Pts',(95.3451403506945,1.24536005250626,-1.26657814105094));
#6985=CARTESIAN_POINT('Ctrl Pts',(95.3440616550468,1.23398505957614,-1.27765203267675));
#6986=CARTESIAN_POINT('Ctrl Pts',(95.3435846090548,1.22890033680306,-1.28254349260462));
#6987=CARTESIAN_POINT('Ctrl Pts',(95.3425111959618,1.21733650987806,-1.29353588048967));
#6988=CARTESIAN_POINT('Ctrl Pts',(95.3419161947615,1.21084055905947,-1.29961855996351));
#6989=CARTESIAN_POINT('Ctrl Pts',(95.340089662298,1.19064337292863,-1.31824790754539));
#6990=CARTESIAN_POINT('Ctrl Pts',(95.3388697170535,1.17679032263864,-1.33062909583091));
#6991=CARTESIAN_POINT('Ctrl Pts',(95.3359971949416,1.14337911723777,-1.3595604051435));
#6992=CARTESIAN_POINT('Ctrl Pts',(95.3343561330884,1.12365180937099,-1.37590953463755));
#6993=CARTESIAN_POINT('Ctrl Pts',(95.3280301460383,1.04544808387427,-1.43791710686284));
#6994=CARTESIAN_POINT('Ctrl Pts',(95.3234763279384,0.984485070895921,-1.48032359163911));
#6995=CARTESIAN_POINT('Ctrl Pts',(95.3117173079998,0.8206856662562,-1.5796566653085));
#6996=CARTESIAN_POINT('Ctrl Pts',(95.3045236388273,0.714552717393068,-1.63041427106398));
#6997=CARTESIAN_POINT('Ctrl Pts',(95.2953923173135,0.581280246780326,-1.67862180093765));
#6998=CARTESIAN_POINT('Ctrl Pts',(95.2938084948094,0.55819782951024,-1.68643795233282));
#6999=CARTESIAN_POINT('Ctrl Pts',(95.2911905369467,0.520160386320609,-1.69845170778107));
#7000=CARTESIAN_POINT('Ctrl Pts',(95.2901656501701,0.505297737654125,-1.70293253006258));
#7001=CARTESIAN_POINT('Ctrl Pts',(95.2883027951456,0.478347950686195,-1.71067354575598));
#7002=CARTESIAN_POINT('Ctrl Pts',(95.2874671097045,0.466281327707187,-1.71400188206105));
#7003=CARTESIAN_POINT('Ctrl Pts',(95.2856573164783,0.440206130705083,-1.72089847978718));
#7004=CARTESIAN_POINT('Ctrl Pts',(95.2846818838194,0.426187240246583,-1.72442379650137));
#7005=CARTESIAN_POINT('Ctrl Pts',(95.2819458810918,0.386973398435257,-1.73377748471631));
#7006=CARTESIAN_POINT('Ctrl Pts',(95.2801733761199,0.361692759244073,-1.73922712799075));
#7007=CARTESIAN_POINT('Ctrl Pts',(95.2724702045185,0.252407513237492,-1.76029960562492));
#7008=CARTESIAN_POINT('Ctrl Pts',(95.2663721128103,0.167465750790382,-1.77039989114934));
#7009=CARTESIAN_POINT('Ctrl Pts',(95.2502794786399,-0.0539681222458069,
-1.78065043690025));
#7010=CARTESIAN_POINT('Ctrl Pts',(95.2401534524402,-0.190348536188963,-1.77127031495713));
#7011=CARTESIAN_POINT('Ctrl Pts',(95.2294194565397,-0.341075672795629,-1.7432790718566));
#7012=CARTESIAN_POINT('Ctrl Pts',(95.2282364246516,-0.357787611082151,-1.73992603745408));
#7013=CARTESIAN_POINT('Ctrl Pts',(95.2264749211728,-0.382858767488722,-1.73451930867552));
#7014=CARTESIAN_POINT('Ctrl Pts',(95.2258872538383,-0.39125502491633,-1.73264467830611));
#7015=CARTESIAN_POINT('Ctrl Pts',(95.2248714263039,-0.405830275616796,-1.72927911123142));
#7016=CARTESIAN_POINT('Ctrl Pts',(95.2244417518351,-0.412015189842297,-1.72781594608054));
#7017=CARTESIAN_POINT('Ctrl Pts',(95.2234246377326,-0.426702631661668,-1.72425798532218));
#7018=CARTESIAN_POINT('Ctrl Pts',(95.2228388937294,-0.435197684934671,-1.72213347883878));
#7019=CARTESIAN_POINT('Ctrl Pts',(95.2210705796401,-0.460941621132549,-1.71549257925249));
#7020=CARTESIAN_POINT('Ctrl Pts',(95.2198985562175,-0.478139116346774,-1.71077906598479));
#7021=CARTESIAN_POINT('Ctrl Pts',(95.2139645498719,-0.565704351290179,-1.68535540345595));
#7022=CARTESIAN_POINT('Ctrl Pts',(95.2093910930455,-0.634818876754864,-1.66055762226319));
#7023=CARTESIAN_POINT('Ctrl Pts',(95.1964484978259,-0.827522332025799,-1.57761952223652));
#7024=CARTESIAN_POINT('Ctrl Pts',(95.1882053118219,-0.946195693212456,-1.50943297655982));
#7025=CARTESIAN_POINT('Ctrl Pts',(95.1773965769074,-1.08192796637439,-1.40909334553449));
#7026=CARTESIAN_POINT('Ctrl Pts',(95.1753002530244,-1.10742900901853,-1.38914108732498));
#7027=CARTESIAN_POINT('Ctrl Pts',(95.1721452626445,-1.14448339748857,-1.35848041529037));
#7028=CARTESIAN_POINT('Ctrl Pts',(95.1711075719997,-1.15646340909492,-1.34829657077988));
#7029=CARTESIAN_POINT('Ctrl Pts',(95.1692310386833,-1.1777459144769,-1.32971262710737));
#7030=CARTESIAN_POINT('Ctrl Pts',(95.1683946341747,-1.1870977852663,-1.32137047951509));
#7031=CARTESIAN_POINT('Ctrl Pts',(95.1665939707368,-1.20693971270538,-1.30329023789246));
#7032=CARTESIAN_POINT('Ctrl Pts',(95.1656285045734,-1.2174018435071,-1.29352295874421));
#7033=CARTESIAN_POINT('Ctrl Pts',(95.1629502542297,-1.24593206827136,-1.2662348676838));
#7034=CARTESIAN_POINT('Ctrl Pts',(95.1612263429251,-1.26374696918884,-1.24845542310128));
#7035=CARTESIAN_POINT('Ctrl Pts',(95.152399111382,-1.3521648206803,-1.15638149238669));
#7036=CARTESIAN_POINT('Ctrl Pts',(95.1450425094611,-1.41660991090255,-1.07646553338749));
#7037=CARTESIAN_POINT('Ctrl Pts',(95.1291959644627,-1.53791981979782,-0.896137958312464));
#7038=CARTESIAN_POINT('Ctrl Pts',(95.1207117506653,-1.59264583236027,-0.794822480818138));
#7039=CARTESIAN_POINT('Ctrl Pts',(95.1111707321944,-1.64521340136675,-0.669897867529944));
#7040=CARTESIAN_POINT('Ctrl Pts',(95.1097315091766,-1.65288882786989,-0.650729516065684));
#7041=CARTESIAN_POINT('Ctrl Pts',(95.107678260501,-1.66349102358425,-0.622853029380883));
#7042=CARTESIAN_POINT('Ctrl Pts',(95.1070500096327,-1.6666869153076,-0.614249963288017));
#7043=CARTESIAN_POINT('Ctrl Pts',(95.1059441935771,-1.67222882539966,-0.59896986072012));
#7044=CARTESIAN_POINT('Ctrl Pts',(95.105465104336,-1.67460181617816,-0.592303049118153));
#7045=CARTESIAN_POINT('Ctrl Pts',(95.1044188508592,-1.67972256448044,-0.577639726472503));
#7046=CARTESIAN_POINT('Ctrl Pts',(95.1038526772859,-1.68245314035489,-0.569637590997079));
#7047=CARTESIAN_POINT('Ctrl Pts',(95.1022038725421,-1.69028172873587,-0.546147945574999));
#7048=CARTESIAN_POINT('Ctrl Pts',(95.1011298050568,-1.69522391876263,-0.530608907419999));
#7049=CARTESIAN_POINT('Ctrl Pts',(95.0937191628379,-1.72814746321451,-0.421933043930216));
#7050=CARTESIAN_POINT('Ctrl Pts',(95.0877332835159,-1.74865625657932,-0.326691590553083));
#7051=CARTESIAN_POINT('Ctrl Pts',(95.0741434425496,-1.7773404623019,-0.10726553706973));
#7052=CARTESIAN_POINT('Ctrl Pts',(95.0665668041369,-1.7804916892154,0.0170396937590265));
#7053=CARTESIAN_POINT('Ctrl Pts',(95.0570192499336,-1.76876145063724,0.164709809400757));
#7054=CARTESIAN_POINT('Ctrl Pts',(95.0554504160024,-1.7663606362436,0.188723087792008));
#7055=CARTESIAN_POINT('Ctrl Pts',(95.0528520911397,-1.76162105744444,0.228022254037951));
#7056=CARTESIAN_POINT('Ctrl Pts',(95.0518316076365,-1.7595705262178,0.24334016606842));
#7057=CARTESIAN_POINT('Ctrl Pts',(95.0499733997698,-1.75549850328728,0.271008562644912));
#7058=CARTESIAN_POINT('Ctrl Pts',(95.0491379047138,-1.75354584950283,0.283368269175139));
#7059=CARTESIAN_POINT('Ctrl Pts',(95.0473246935836,-1.74904765090326,0.310011037129568));
#7060=CARTESIAN_POINT('Ctrl Pts',(95.0463456100258,-1.74645738825423,0.324285518475907));
#7061=CARTESIAN_POINT('Ctrl Pts',(95.0435883381943,-1.73871557095237,0.364162329949569));
#7062=CARTESIAN_POINT('Ctrl Pts',(95.0417979111599,-1.73317400411456,0.389684210974678));
#7063=CARTESIAN_POINT('Ctrl Pts',(95.0339428759946,-1.70666171999534,0.499998706699272));
#7064=CARTESIAN_POINT('Ctrl Pts',(95.0277028843341,-1.68001816416497,0.583290644364273));
#7065=CARTESIAN_POINT('Ctrl Pts',(95.0117066079709,-1.59767699582025,0.787491680522473));
#7066=CARTESIAN_POINT('Ctrl Pts',(95.0018426481373,-1.53432409620246,0.904747022041888));
#7067=CARTESIAN_POINT('Ctrl Pts',(94.9912894596819,-1.44838529901362,1.02837604788023));
#7068=CARTESIAN_POINT('Ctrl Pts',(94.990059980716,-1.43806675187335,1.04275660960599));
#7069=CARTESIAN_POINT('Ctrl Pts',(94.9882438534851,-1.42233915655661,1.06399793819069));
#7070=CARTESIAN_POINT('Ctrl Pts',(94.9876471802424,-1.4170919966957,1.07097645620828));
#7071=CARTESIAN_POINT('Ctrl Pts',(94.9865746236708,-1.4075107247553,1.08352546255025));
#7072=CARTESIAN_POINT('Ctrl Pts',(94.9860975810893,-1.40319468065931,1.0891090672964));
#7073=CARTESIAN_POINT('Ctrl Pts',(94.9850179752984,-1.39330297239163,1.10174941113212));
#7074=CARTESIAN_POINT('Ctrl Pts',(94.9844168555606,-1.38770686901168,1.10878969702321));
#7075=CARTESIAN_POINT('Ctrl Pts',(94.9825511889574,-1.37007076034943,1.13063446331415));
#7076=CARTESIAN_POINT('Ctrl Pts',(94.9812989542025,-1.35784506876156,1.14528818177321));
#7077=CARTESIAN_POINT('Ctrl Pts',(94.9783350577334,-1.32804496998012,1.17985843991184));
#7078=CARTESIAN_POINT('Ctrl Pts',(94.9766359253695,-1.31025504095858,1.19958378468223));
#7079=CARTESIAN_POINT('Ctrl Pts',(94.969934113325,-1.2375955262759,1.27660230793023));
#7080=CARTESIAN_POINT('Ctrl Pts',(94.965078843049,-1.17935497475244,1.33059372196977));
#7081=CARTESIAN_POINT('Ctrl Pts',(94.9534424500203,-1.03201372128253,1.44988470252031));
#7082=CARTESIAN_POINT('Ctrl Pts',(94.9466620620704,-0.940068495925,1.5111206372368));
#7083=CARTESIAN_POINT('Ctrl Pts',(94.9379825175937,-0.821473912657809,1.57506995714734));
#7084=CARTESIAN_POINT('Ctrl Pts',(94.936389783875,-0.79966367959214,1.5862542876717));
#7085=CARTESIAN_POINT('Ctrl Pts',(94.9337601581515,-0.763636625949545,1.60379718300328));
#7086=CARTESIAN_POINT('Ctrl Pts',(94.9327326594191,-0.749554841324666,1.61042659404732));
#7087=CARTESIAN_POINT('Ctrl Pts',(94.9308670335171,-0.723991625699923,1.62205330861708));
#7088=CARTESIAN_POINT('Ctrl Pts',(94.9300312208673,-0.712540902645496,1.62711593266471));
#7089=CARTESIAN_POINT('Ctrl Pts',(94.9282233853606,-0.687783848757428,1.6377501399672));
#7090=CARTESIAN_POINT('Ctrl Pts',(94.9272500623634,-0.674461325399115,1.64328148614164));
#7091=CARTESIAN_POINT('Ctrl Pts',(94.9245263212566,-0.637207859443691,1.65821932763941));
#7092=CARTESIAN_POINT('Ctrl Pts',(94.9227641418537,-0.613138655464252,1.6672690434214));
#7093=CARTESIAN_POINT('Ctrl Pts',(94.915147377191,-0.509293203912989,1.70376089238181));
#7094=CARTESIAN_POINT('Ctrl Pts',(94.9091298018082,-0.427823702698999,1.72601971223949));
#7095=CARTESIAN_POINT('Ctrl Pts',(94.8945833023764,-0.23118032335632,1.76496585089555));
#7096=CARTESIAN_POINT('Ctrl Pts',(94.8859871579056,-0.11533655142876,1.77630087991323));
#7097=CARTESIAN_POINT('Ctrl Pts',(94.877703379636,0.000780936357206753,
1.77624982832889));
#7098=CARTESIAN_POINT('Ctrl Pts',(94.8777032004959,0.000783447447140647,
1.7762498272231));
#7099=CARTESIAN_POINT('Ctrl Pts',(94.875703743125,0.0288107681561156,1.77623746526111));
#7100=CARTESIAN_POINT('Ctrl Pts',(94.8737250593201,0.0568359658703815,1.77556174085671));
#7101=CARTESIAN_POINT('Ctrl Pts',(94.8710993587005,0.0945567494872465,1.77375810203675));
#7102=CARTESIAN_POINT('Ctrl Pts',(94.870426291296,0.10427439127338,1.77321336702983));
#7103=CARTESIAN_POINT('Ctrl Pts',(94.8692666882143,0.121108806098811,1.77213082045504));
#7104=CARTESIAN_POINT('Ctrl Pts',(94.8687783067807,0.128227617541035,1.77162994730939));
#7105=CARTESIAN_POINT('Ctrl Pts',(94.8678277550067,0.142143366094598,1.77056652966511));
#7106=CARTESIAN_POINT('Ctrl Pts',(94.8673654011623,0.148940475069296,1.77000771579285));
#7107=CARTESIAN_POINT('Ctrl Pts',(94.8663652577609,0.163708107271948,1.76870794332323));
#7108=CARTESIAN_POINT('Ctrl Pts',(94.8658282854875,0.171677059085947,1.76795224111264));
#7109=CARTESIAN_POINT('Ctrl Pts',(94.8643505085288,0.193710050634295,1.76571245320849));
#7110=CARTESIAN_POINT('Ctrl Pts',(94.8634157709342,0.207762242826518,1.76411420625861));
#7111=CARTESIAN_POINT('Ctrl Pts',(94.8586703207988,0.279595805800326,1.75507383565549));
#7112=CARTESIAN_POINT('Ctrl Pts',(94.8549859291996,0.337010668443167,1.74495937527194));
#7113=CARTESIAN_POINT('Ctrl Pts',(94.84421111473,0.505731147393458,1.70659583264059));
#7114=CARTESIAN_POINT('Ctrl Pts',(94.8372918228665,0.614903438240659,1.67036769308429));
#7115=CARTESIAN_POINT('Ctrl Pts',(94.8260972895909,0.778940256290118,1.59765394461424));
#7116=CARTESIAN_POINT('Ctrl Pts',(94.8219990014537,0.836579443054001,1.5682408995006));
#7117=CARTESIAN_POINT('Ctrl Pts',(94.8164896090179,0.90978577643737,1.52569800683077));
#7118=CARTESIAN_POINT('Ctrl Pts',(94.8151776146235,0.926916987703905,1.51535125028546));
#7119=CARTESIAN_POINT('Ctrl Pts',(94.8129802009186,0.955083961327412,1.4976828596905));
#7120=CARTESIAN_POINT('Ctrl Pts',(94.8121007696611,0.96621948330322,1.49052313479004));
#7121=CARTESIAN_POINT('Ctrl Pts',(94.8103651199301,0.987921238072749,1.47622433141034));
#7122=CARTESIAN_POINT('Ctrl Pts',(94.809509289856,0.998492694527664,1.46909461014019));
#7123=CARTESIAN_POINT('Ctrl Pts',(94.8076161708394,1.02158779773059,1.45315411566405));
#7124=CARTESIAN_POINT('Ctrl Pts',(94.806577045216,1.0340760059473,1.44429404921418));
#7125=CARTESIAN_POINT('Ctrl Pts',(94.802998916464,1.07642500819074,1.41341769880217));
#7126=CARTESIAN_POINT('Ctrl Pts',(94.8004304361012,1.10570805280832,1.39062925916566));
#7127=CARTESIAN_POINT('Ctrl Pts',(94.7886790829253,1.23464563109819,1.28364008405797));
#7128=CARTESIAN_POINT('Ctrl Pts',(94.7791128656865,1.32554221729754,1.18954188861098));
#7129=CARTESIAN_POINT('Ctrl Pts',(94.764381381594,1.44896646288052,1.02988187557092));
#7130=CARTESIAN_POINT('Ctrl Pts',(94.7592062256311,1.48918810011262,0.970814732654317));
#7131=CARTESIAN_POINT('Ctrl Pts',(94.7529674294456,1.53476904779362,0.894348050746785));
#7132=CARTESIAN_POINT('Ctrl Pts',(94.7517435890676,1.5435647888861,0.87908035308186));
#7133=CARTESIAN_POINT('Ctrl Pts',(94.7499340809887,1.55637005957131,0.856067904802723));
#7134=CARTESIAN_POINT('Ctrl Pts',(94.7493384906121,1.56055181923945,0.848420914107435));
#7135=CARTESIAN_POINT('Ctrl Pts',(94.748314815403,1.56768464611979,0.835146264809442));
#7136=CARTESIAN_POINT('Ctrl Pts',(94.7478851241269,1.57066197592887,0.829533238696455));
#7137=CARTESIAN_POINT('Ctrl Pts',(94.7468755652192,1.57761741955346,0.81624874218973));
#7138=CARTESIAN_POINT('Ctrl Pts',(94.7462973013654,1.58156974962538,0.808564076914775));
#7139=CARTESIAN_POINT('Ctrl Pts',(94.7446107894178,1.59299710025869,0.785941038893312));
#7140=CARTESIAN_POINT('Ctrl Pts',(94.7435115015725,1.60031790311815,0.770925247035328));
#7141=CARTESIAN_POINT('Ctrl Pts',(94.7350147950301,1.65577918666664,0.652972084690577));
#7142=CARTESIAN_POINT('Ctrl Pts',(94.7280933940864,1.69415909453756,0.545719051896373));
#7143=CARTESIAN_POINT('Ctrl Pts',(94.714985142822,1.74651125830193,0.33872130499129));
#7144=CARTESIAN_POINT('Ctrl Pts',(94.7088334531639,1.76278532830978,0.240039130214569));
#7145=CARTESIAN_POINT('Ctrl Pts',(94.7004472569654,1.77312909141282,0.109696185932724));
#7146=CARTESIAN_POINT('Ctrl Pts',(94.6984427640807,1.77476974884387,0.0788173959524371));
#7147=CARTESIAN_POINT('Ctrl Pts',(94.6953990870834,1.77602050079453,0.0324658310265796));
#7148=CARTESIAN_POINT('Ctrl Pts',(94.6943787048488,1.77623572074468,0.0170143637278835));
#7149=CARTESIAN_POINT('Ctrl Pts',(94.6925206034954,1.77626031955146,-0.0109503858670986));
#7150=CARTESIAN_POINT('Ctrl Pts',(94.6916851124531,1.77613910528311,-0.0234627078840527));
#7151=CARTESIAN_POINT('Ctrl Pts',(94.6905865700469,1.7758075807968,-0.0398293953416206));
#7152=CARTESIAN_POINT('Ctrl Pts',(94.6903272973286,1.77571689021663,-0.0436860354302763));
#7153=CARTESIAN_POINT('Ctrl Pts',(94.6900676319115,1.77561363837053,-0.0475422941449777));
#7154=CARTESIAN_POINT('Ctrl Pts',(94.5412649413994,1.77561364082571,-0.0475422024484629));
#7155=CARTESIAN_POINT('Ctrl Pts',(94.5434435753088,1.77655815902118,-0.0122661886016114));
#7156=CARTESIAN_POINT('Ctrl Pts',(94.5456095196027,1.77645169809017,0.0230475721265798));
#7157=CARTESIAN_POINT('Ctrl Pts',(94.5527068568138,1.77265305223877,0.13861651702398));
#7158=CARTESIAN_POINT('Ctrl Pts',(94.5576379267421,1.76457463705705,0.218606026469179));
#7159=CARTESIAN_POINT('Ctrl Pts',(94.5657720795508,1.74295772007151,0.345729776074744));
#7160=CARTESIAN_POINT('Ctrl Pts',(94.5688853545426,1.73283620115693,0.393330323373668));
#7161=CARTESIAN_POINT('Ctrl Pts',(94.5732511454832,1.71624881524957,0.458134480433476));
#7162=CARTESIAN_POINT('Ctrl Pts',(94.5744506205441,1.71145078563001,0.475745063641914));
#7163=CARTESIAN_POINT('Ctrl Pts',(94.5765125960301,1.70280106133474,0.505666802134386));
#7164=CARTESIAN_POINT('Ctrl Pts',(94.5773706405815,1.69908501689463,0.518015887451013));
#7165=CARTESIAN_POINT('Ctrl Pts',(94.5790149050942,1.69174492462631,0.541479281216473));
#7166=CARTESIAN_POINT('Ctrl Pts',(94.5798002946744,1.68814496518447,0.552600458880006));
#7167=CARTESIAN_POINT('Ctrl Pts',(94.5816516457733,1.67944135714042,0.578609072298788));
#7168=CARTESIAN_POINT('Ctrl Pts',(94.5827204840958,1.67424916718845,0.593465608874096));
#7169=CARTESIAN_POINT('Ctrl Pts',(94.5865124798222,1.6552470192782,0.645601887097282));
#7170=CARTESIAN_POINT('Ctrl Pts',(94.5892699932211,1.64038456002125,0.682482638773605));
#7171=CARTESIAN_POINT('Ctrl Pts',(94.6010434200455,1.57262699252526,0.83559018769827));
#7172=CARTESIAN_POINT('Ctrl Pts',(94.6104123635189,1.50852229504532,0.946424030956493));
#7173=CARTESIAN_POINT('Ctrl Pts',(94.6235364062967,1.40228318021252,1.09150726091316));
#7174=CARTESIAN_POINT('Ctrl Pts',(94.6273238652075,1.36961682322703,1.1322264051728));
#7175=CARTESIAN_POINT('Ctrl Pts',(94.6325255392511,1.32144277379587,1.18713453414243));
#7176=CARTESIAN_POINT('Ctrl Pts',(94.6339994282064,1.30740627510489,1.20257570203997));
#7177=CARTESIAN_POINT('Ctrl Pts',(94.6365701166745,1.2821876951167,1.22935435805946));
#7178=CARTESIAN_POINT('Ctrl Pts',(94.6376733263133,1.27111931151023,1.24079537525619));
#7179=CARTESIAN_POINT('Ctrl Pts',(94.6393404165796,1.25399393429083,1.25802759555352));
#7180=CARTESIAN_POINT('Ctrl Pts',(94.6399121397877,1.2480476146365,1.26392696672909));
#7181=CARTESIAN_POINT('Ctrl Pts',(94.6409614888597,1.23699376369573,1.27473946701458));
#7182=CARTESIAN_POINT('Ctrl Pts',(94.6414399693347,1.2318984362493,1.27966422375792));
#7183=CARTESIAN_POINT('Ctrl Pts',(94.642540041456,1.22005809701332,1.29097193205022));
#7184=CARTESIAN_POINT('Ctrl Pts',(94.6431599607674,1.21329233301522,1.2973326534049));
#7185=CARTESIAN_POINT('Ctrl Pts',(94.6451883213664,1.19085916085582,1.31809382820894));
#7186=CARTESIAN_POINT('Ctrl Pts',(94.6465809711968,1.17498219071284,1.33226642609027));
#7187=CARTESIAN_POINT('Ctrl Pts',(94.6564081460819,1.05988575192336,1.4313488550651));
#7188=CARTESIAN_POINT('Ctrl Pts',(94.6642639264257,0.951812226279923,1.50538350037581));
#7189=CARTESIAN_POINT('Ctrl Pts',(94.6775415222494,0.761795526559401,1.60683530918759));
#7190=CARTESIAN_POINT('Ctrl Pts',(94.6828276127812,0.684250487879997,1.64135646493972));
#7191=CARTESIAN_POINT('Ctrl Pts',(94.689961140598,0.580311036885342,1.67897804010269));
#7192=CARTESIAN_POINT('Ctrl Pts',(94.6916397317116,0.555892524882368,1.68722006550244));
#7193=CARTESIAN_POINT('Ctrl Pts',(94.6942857863076,0.517528764756738,1.69924584836991));
#7194=CARTESIAN_POINT('Ctrl Pts',(94.6952412464933,0.503701418451321,1.70339582478594));
#7195=CARTESIAN_POINT('Ctrl Pts',(94.6970355597131,0.477792442568631,1.71082879107591));
#7196=CARTESIAN_POINT('Ctrl Pts',(94.6978729907988,0.465723642820633,1.71415350689919));
#7197=CARTESIAN_POINT('Ctrl Pts',(94.6997598697513,0.438589493482345,1.72132072206722));
#7198=CARTESIAN_POINT('Ctrl Pts',(94.700811502654,0.423506969534449,1.72509350236888));
#7199=CARTESIAN_POINT('Ctrl Pts',(94.7035336668793,0.384580720599134,1.73428936766983));
#7200=CARTESIAN_POINT('Ctrl Pts',(94.7052133781941,0.360671714155253,1.73941879735231));
#7201=CARTESIAN_POINT('Ctrl Pts',(94.7147798457699,0.225174148445743,1.76557474098718));
#7202=CARTESIAN_POINT('Ctrl Pts',(94.7229820693175,0.111894069949005,1.77635281458003));
#7203=CARTESIAN_POINT('Ctrl Pts',(94.7389518392365,-0.106611507095988,1.77615348264895));
#7204=CARTESIAN_POINT('Ctrl Pts',(94.746668989523,-0.211395605660704,1.76674918023911));
#7205=CARTESIAN_POINT('Ctrl Pts',(94.7552634553239,-0.332087971155573,1.74501927664064));
#7206=CARTESIAN_POINT('Ctrl Pts',(94.7564877600887,-0.349387274758901,1.7416381046173));
#7207=CARTESIAN_POINT('Ctrl Pts',(94.7582978003044,-0.375162915506406,1.73620068701901));
#7208=CARTESIAN_POINT('Ctrl Pts',(94.7588934669821,-0.383678520159998,1.73433873277692));
#7209=CARTESIAN_POINT('Ctrl Pts',(94.7599650217581,-0.399063629366382,1.73085588382814));
#7210=CARTESIAN_POINT('Ctrl Pts',(94.7604420572206,-0.40593748644609,1.72925667033796));
#7211=CARTESIAN_POINT('Ctrl Pts',(94.7615226513983,-0.421563592899136,1.72552292000326));
#7212=CARTESIAN_POINT('Ctrl Pts',(94.7621247540477,-0.430309341109339,1.72336272735353));
#7213=CARTESIAN_POINT('Ctrl Pts',(94.7639968300216,-0.457608564069119,1.71639906499678));
#7214=CARTESIAN_POINT('Ctrl Pts',(94.7652543697975,-0.476101663996281,1.71136162943988));
#7215=CARTESIAN_POINT('Ctrl Pts',(94.768233372978,-0.520168319588268,1.6985884189086));
#7216=CARTESIAN_POINT('Ctrl Pts',(94.7699421344828,-0.545656460626269,1.6905729428433));
#7217=CARTESIAN_POINT('Ctrl Pts',(94.7767083201064,-0.646906959570245,1.65620312853243));
#7218=CARTESIAN_POINT('Ctrl Pts',(94.7816154567932,-0.721030108955061,1.62530449470644));
#7219=CARTESIAN_POINT('Ctrl Pts',(94.7932330923504,-0.890396752790922,1.54082733611291));
#7220=CARTESIAN_POINT('Ctrl Pts',(94.7999437074288,-0.983278404503882,1.48327855500644));
#7221=CARTESIAN_POINT('Ctrl Pts',(94.8085468900542,-1.08986526937704,1.4028040514305));
#7222=CARTESIAN_POINT('Ctrl Pts',(94.8101405954477,-1.10912869219456,1.38762349454655));
#7223=CARTESIAN_POINT('Ctrl Pts',(94.81277147336,-1.14009642816649,1.36216245883458));
#7224=CARTESIAN_POINT('Ctrl Pts',(94.8137992365312,-1.15199107933619,1.35211795238197));
#7225=CARTESIAN_POINT('Ctrl Pts',(94.8156651144676,-1.17321025229277,1.3337160531245));
#7226=CARTESIAN_POINT('Ctrl Pts',(94.8165009112172,-1.1825814461775,1.32541386585446));
#7227=CARTESIAN_POINT('Ctrl Pts',(94.8183084541581,-1.20255644791122,1.30733699456991));
#7228=CARTESIAN_POINT('Ctrl Pts',(94.8192814975433,-1.21313048100066,1.2975309023102));
#7229=CARTESIAN_POINT('Ctrl Pts',(94.8220037216389,-1.24220958108485,1.26989748804954));
#7230=CARTESIAN_POINT('Ctrl Pts',(94.8237646428141,-1.26044833168126,1.2517963716943));
#7231=CARTESIAN_POINT('Ctrl Pts',(94.8313711261778,-1.33677242489935,1.17268863172378));
#7232=CARTESIAN_POINT('Ctrl Pts',(94.8373791575991,-1.39086350194149,1.10799562186814));
#7233=CARTESIAN_POINT('Ctrl Pts',(94.8527475346567,-1.51483987673093,0.936270947243736));
#7234=CARTESIAN_POINT('Ctrl Pts',(94.8622145351851,-1.57816049923806,0.825078083531655));
#7235=CARTESIAN_POINT('Ctrl Pts',(94.8728821540885,-1.63831439447118,0.686682823221446));
#7236=CARTESIAN_POINT('Ctrl Pts',(94.8745129533067,-1.64718470709737,0.665124065403948));
#7237=CARTESIAN_POINT('Ctrl Pts',(94.8767467116256,-1.6589098163154,0.634952236839583));
#7238=CARTESIAN_POINT('Ctrl Pts',(94.8773684449951,-1.66212650423166,0.626483530869504));
#7239=CARTESIAN_POINT('Ctrl Pts',(94.8784792478827,-1.66779130427911,0.611218780106395));
#7240=CARTESIAN_POINT('Ctrl Pts',(94.8789696540811,-1.6702630139578,0.604431719198467));
#7241=CARTESIAN_POINT('Ctrl Pts',(94.879978543617,-1.67528848118149,0.590366039129934));
#7242=CARTESIAN_POINT('Ctrl Pts',(94.8804966876522,-1.67783634156848,0.583085561431611));
#7243=CARTESIAN_POINT('Ctrl Pts',(94.8818671320378,-1.68448380497436,0.563686118329876));
#7244=CARTESIAN_POINT('Ctrl Pts',(94.8827147370964,-1.68850013209264,0.551538807908548));
#7245=CARTESIAN_POINT('Ctrl Pts',(94.88701432694,-1.70835896923778,0.489225139120706));
#7246=CARTESIAN_POINT('Ctrl Pts',(94.8903609323159,-1.72209994049072,0.438411365064706));
#7247=CARTESIAN_POINT('Ctrl Pts',(94.9036857741804,-1.76849888945552,0.230598326965006));
#7248=CARTESIAN_POINT('Ctrl Pts',(94.9132243868449,-1.78209093110531,0.0701343464581758));
#7249=CARTESIAN_POINT('Ctrl Pts',(94.9257522701928,-1.77214205701239,-0.126007263530086));
#7250=CARTESIAN_POINT('Ctrl Pts',(94.9280811972879,-1.76921778330781,-0.161967437868291));
#7251=CARTESIAN_POINT('Ctrl Pts',(94.9315050673402,-1.7633968524475,-0.21391131945955));
#7252=CARTESIAN_POINT('Ctrl Pts',(94.9325728633011,-1.7613725929161,-0.229984938382008));
#7253=CARTESIAN_POINT('Ctrl Pts',(94.9344843034777,-1.75738192392362,-0.258518663800589));
#7254=CARTESIAN_POINT('Ctrl Pts',(94.9353251626267,-1.75550209055475,-0.270989892894573));
#7255=CARTESIAN_POINT('Ctrl Pts',(94.9371000712876,-1.75127545796363,-0.297137798532043));
#7256=CARTESIAN_POINT('Ctrl Pts',(94.9380349504658,-1.74890088713878,-0.310809055377591));
#7257=CARTESIAN_POINT('Ctrl Pts',(94.9405382663113,-1.74215142742212,-0.347138235356091));
#7258=CARTESIAN_POINT('Ctrl Pts',(94.9421155343129,-1.73749488418756,-0.369740436532594));
#7259=CARTESIAN_POINT('Ctrl Pts',(94.9519300734694,-1.70606385045465,-0.508559700312585));
#7260=CARTESIAN_POINT('Ctrl Pts',(94.9605275135835,-1.66808572455898,-0.621906143790832));
#7261=CARTESIAN_POINT('Ctrl Pts',(94.9770561318937,-1.57505260064922,-0.828080069001339));
#7262=CARTESIAN_POINT('Ctrl Pts',(94.9849239146365,-1.52233277957435,-0.921419479417054));
#7263=CARTESIAN_POINT('Ctrl Pts',(94.9936347948144,-1.45166570501596,-1.02373434210288));
#7264=CARTESIAN_POINT('Ctrl Pts',(94.9948400755776,-1.44159244751381,-1.03787118367639));
#7265=CARTESIAN_POINT('Ctrl Pts',(94.9966277598574,-1.42618238120057,-1.0588403779074));
#7266=CARTESIAN_POINT('Ctrl Pts',(94.9972197526479,-1.42100048785081,-1.06578457100507));
#7267=CARTESIAN_POINT('Ctrl Pts',(94.9982397279222,-1.41193145563184,-1.07775413845314));
#7268=CARTESIAN_POINT('Ctrl Pts',(94.9986692760981,-1.40806797023224,-1.08279684743485));
#7269=CARTESIAN_POINT('Ctrl Pts',(94.9996819527362,-1.3988548921779,-1.09468926274514));
#7270=CARTESIAN_POINT('Ctrl Pts',(95.0002634368031,-1.3934819848297,-1.10152056595514));
#7271=CARTESIAN_POINT('Ctrl Pts',(95.0020054073728,-1.37714420552958,-1.12198212815959));
#7272=CARTESIAN_POINT('Ctrl Pts',(95.003155801247,-1.36602755333219,-1.13549057186784));
#7273=CARTESIAN_POINT('Ctrl Pts',(95.0088694110335,-1.30927830354811,-1.20240970909248));
#7274=CARTESIAN_POINT('Ctrl Pts',(95.0132593202433,-1.26070049116031,-1.25324985570592));
#7275=CARTESIAN_POINT('Ctrl Pts',(95.0254475237736,-1.11616753847906,-1.38757954873728));
#7276=CARTESIAN_POINT('Ctrl Pts',(95.033121635433,-1.01409527658672,-1.46383623508831));
#7277=CARTESIAN_POINT('Ctrl Pts',(95.0437489087865,-0.87001800323518,-1.54911679932686));
#7278=CARTESIAN_POINT('Ctrl Pts',(95.0463448859884,-0.834584722617513,-1.56849040086878));
#7279=CARTESIAN_POINT('Ctrl Pts',(95.0500169875117,-0.784389482339222,-1.5937526773605));
#7280=CARTESIAN_POINT('Ctrl Pts',(95.0510572721582,-0.770160762154759,-1.60067699127721));
#7281=CARTESIAN_POINT('Ctrl Pts',(95.0528788410603,-0.745245153024947,-1.61239289303791));
#7282=CARTESIAN_POINT('Ctrl Pts',(95.053657105732,-0.734599715248548,-1.61727067208922));
#7283=CARTESIAN_POINT('Ctrl Pts',(95.0552988179213,-0.712148975299129,-1.62729029012666));
#7284=CARTESIAN_POINT('Ctrl Pts',(95.0561629772106,-0.700334476037257,-1.63240970895281));
#7285=CARTESIAN_POINT('Ctrl Pts',(95.0582553817403,-0.671742383278715,-1.64443161667852));
#7286=CARTESIAN_POINT('Ctrl Pts',(95.0594878620959,-0.654912963943813,-1.65120626767301));
#7287=CARTESIAN_POINT('Ctrl Pts',(95.0639998206859,-0.593367912671106,-1.67489221659939));
#7288=CARTESIAN_POINT('Ctrl Pts',(95.0673296359578,-0.54808159029031,-1.69025301140629));
#7289=CARTESIAN_POINT('Ctrl Pts',(95.0762308901081,-0.427409082755968,-1.72582469587156));
#7290=CARTESIAN_POINT('Ctrl Pts',(95.0818829023581,-0.351219060787104,-1.74292638970081));
#7291=CARTESIAN_POINT('Ctrl Pts',(95.0956950600995,-0.164373503566121,-1.7721152392473));
#7292=CARTESIAN_POINT('Ctrl Pts',(95.1038795333791,-0.0532130267965422,
-1.77892754413776));
#7293=CARTESIAN_POINT('Ctrl Pts',(95.1128575780263,0.0749361269299614,-1.77475082035718));
#7294=CARTESIAN_POINT('Ctrl Pts',(95.1140434384957,0.0920021229135656,-1.77394801522403));
#7295=CARTESIAN_POINT('Ctrl Pts',(95.1158082619779,0.117648740364889,-1.77237043935367));
#7296=CARTESIAN_POINT('Ctrl Pts',(95.116396470495,0.126239103854104,-1.77177930252482));
#7297=CARTESIAN_POINT('Ctrl Pts',(95.117412798325,0.141161734065333,-1.77064333324257));
#7298=CARTESIAN_POINT('Ctrl Pts',(95.1178424384907,0.147495688575089,-1.77012696540166));
#7299=CARTESIAN_POINT('Ctrl Pts',(95.1188589253252,0.162541516793648,-1.76881905046448));
#7300=CARTESIAN_POINT('Ctrl Pts',(95.1194440832824,0.171250480059544,-1.76799713210154));
#7301=CARTESIAN_POINT('Ctrl Pts',(95.121208817696,0.19764592661323,-1.76530915916036));
#7302=CARTESIAN_POINT('Ctrl Pts',(95.1223779094459,0.215311383646996,-1.7632417324343));
#7303=CARTESIAN_POINT('Ctrl Pts',(95.1282817616309,0.305238573714238,-1.75134562496465));
#7304=CARTESIAN_POINT('Ctrl Pts',(95.1328301145104,0.376884303222874,-1.73733780508449));
#7305=CARTESIAN_POINT('Ctrl Pts',(95.1456670787031,0.578221806123637,-1.68492652615933));
#7306=CARTESIAN_POINT('Ctrl Pts',(95.1538297663241,0.70465086388769,-1.63608765895191));
#7307=CARTESIAN_POINT('Ctrl Pts',(95.1645894126931,0.853676717625577,-1.55801106405439));
#7308=CARTESIAN_POINT('Ctrl Pts',(95.166733008376,0.882595328091569,-1.54181311344165));
#7309=CARTESIAN_POINT('Ctrl Pts',(95.1699593513328,0.924850222355441,-1.51656679347856));
#7310=CARTESIAN_POINT('Ctrl Pts',(95.1710201463706,0.938544807379738,-1.50813009687887));
#7311=CARTESIAN_POINT('Ctrl Pts',(95.1729218754768,0.962730480610808,-1.49277325131496));
#7312=CARTESIAN_POINT('Ctrl Pts',(95.1737600907851,0.973266381157452,-1.48592546768418));
#7313=CARTESIAN_POINT('Ctrl Pts',(95.1755468440813,0.995456352245029,-1.4711659004954));
#7314=CARTESIAN_POINT('Ctrl Pts',(95.1764963968491,1.00709068531736,-1.4632261573744));
#7315=CARTESIAN_POINT('Ctrl Pts',(95.1790833471573,1.0383520440042,-1.44134267528383));
#7316=CARTESIAN_POINT('Ctrl Pts',(95.1807306461126,1.05779138225488,-1.42713733299095));
#7317=CARTESIAN_POINT('Ctrl Pts',(95.1844334598677,1.10043622175063,-1.39462450664985));
#7318=CARTESIAN_POINT('Ctrl Pts',(95.1864960078317,1.12348517127626,-1.37612437235903));
#7319=CARTESIAN_POINT('Ctrl Pts',(95.1932713126165,1.1969259695372,-1.31410228372658));
#7320=CARTESIAN_POINT('Ctrl Pts',(95.1980634804437,1.24533103709929,-1.26832396499313));
#7321=CARTESIAN_POINT('Ctrl Pts',(95.2102229721831,1.36010362625739,-1.14686153849779));
#7322=CARTESIAN_POINT('Ctrl Pts',(95.2176419270819,1.42282901537072,-1.06805032390844));
#7323=CARTESIAN_POINT('Ctrl Pts',(95.2275189585559,1.49919773066883,-0.953340656220574));
#7324=CARTESIAN_POINT('Ctrl Pts',(95.2301563675644,1.51886618126048,-0.921682275466301));
#7325=CARTESIAN_POINT('Ctrl Pts',(95.2335640464393,1.54347746721085,-0.879137448296057));
#7326=CARTESIAN_POINT('Ctrl Pts',(95.2343825668173,1.54932606729685,-0.868788870410129));
#7327=CARTESIAN_POINT('Ctrl Pts',(95.235708401415,1.55870284709006,-0.851801615550708));
#7328=CARTESIAN_POINT('Ctrl Pts',(95.2362194709419,1.56229343614907,-0.845198072931727));
#7329=CARTESIAN_POINT('Ctrl Pts',(95.2372323281931,1.56936369097838,-0.831995980060367));
#7330=CARTESIAN_POINT('Ctrl Pts',(95.2377341406856,1.57284391557293,-0.825397920617801));
#7331=CARTESIAN_POINT('Ctrl Pts',(95.2390112958784,1.58163952950383,-0.808464914562898));
#7332=CARTESIAN_POINT('Ctrl Pts',(95.2397830249633,1.58689535073497,-0.798099168716691));
#7333=CARTESIAN_POINT('Ctrl Pts',(95.2430663341115,1.6089794240698,-0.753463235619792));
#7334=CARTESIAN_POINT('Ctrl Pts',(95.2455233506389,1.6248034083339,-0.718704390900775));
#7335=CARTESIAN_POINT('Ctrl Pts',(95.252726840723,1.66854897756847,-0.613766708088673));
#7336=CARTESIAN_POINT('Ctrl Pts',(95.2573583214528,1.69313063363843,-0.542287244323431));
#7337=CARTESIAN_POINT('Ctrl Pts',(95.2690837777104,1.74361902570175,-0.358050339677971));
#7338=CARTESIAN_POINT('Ctrl Pts',(95.2761699902226,1.76320571122477,-0.24394500650331));
#7339=CARTESIAN_POINT('Ctrl Pts',(95.2851838045764,1.77334698114173,-0.104405221888593));
#7340=CARTESIAN_POINT('Ctrl Pts',(95.2867703384516,1.77461426961264,-0.0800254182370063));
#7341=CARTESIAN_POINT('Ctrl Pts',(95.2885492368346,1.77546315899532,-0.0529330183040422));
#7342=CARTESIAN_POINT('Ctrl Pts',(95.2887263841943,1.77554146783561,-0.050237725415923));
#7343=CARTESIAN_POINT('Ctrl Pts',(95.2889037169497,1.77561363837295,-0.0475422940546111));
#7344=CARTESIAN_POINT('Origin',(88.3562164250559,0.,0.));
#7345=CARTESIAN_POINT('',(96.1869838792616,1.77561363799551,-0.0475423081512957));
#7346=CARTESIAN_POINT('',(96.0403469459233,1.77561363956144,-0.0475422496666916));
#7347=CARTESIAN_POINT('',(88.3562164250559,1.77561363837197,-0.0475422940912398));
#7348=CARTESIAN_POINT('Ctrl Pts',(96.1869838792616,1.77561363799551,-0.0475423081512957));
#7349=CARTESIAN_POINT('Ctrl Pts',(96.1859735229126,1.77523265929886,-0.0617711286663794));
#7350=CARTESIAN_POINT('Ctrl Pts',(96.1849689213711,1.77468059977411,-0.0759971484777021));
#7351=CARTESIAN_POINT('Ctrl Pts',(96.1827450801735,1.77306860399109,-0.107694088353561));
#7352=CARTESIAN_POINT('Ctrl Pts',(96.1815296802457,1.77192153164029,-0.125157638420296));
#7353=CARTESIAN_POINT('Ctrl Pts',(96.1797300866637,1.76981866583316,-0.151266345408754));
#7354=CARTESIAN_POINT('Ctrl Pts',(96.1791361226274,1.7690572234074,-0.159925499836574));
#7355=CARTESIAN_POINT('Ctrl Pts',(96.178114144888,1.76762928885563,-0.174903170570591));
#7356=CARTESIAN_POINT('Ctrl Pts',(96.1776845429653,1.76699243626332,-0.181224047609109));
#7357=CARTESIAN_POINT('Ctrl Pts',(96.1766736081873,1.76540694149744,-0.196156692790316));
#7358=CARTESIAN_POINT('Ctrl Pts',(96.1760938975564,1.76442919360367,-0.204765099153601));
#7359=CARTESIAN_POINT('Ctrl Pts',(96.1743989621701,1.76136919100643,-0.230054824132373));
#7360=CARTESIAN_POINT('Ctrl Pts',(96.1732928321384,1.75911300867986,-0.246714657494879));
#7361=CARTESIAN_POINT('Ctrl Pts',(96.1648781519479,1.73997177847874,-0.374396708413501));
#7362=CARTESIAN_POINT('Ctrl Pts',(96.1580333729285,1.71282649337141,-0.483639263159261));
#7363=CARTESIAN_POINT('Ctrl Pts',(96.1492357523241,1.66525661782863,-0.618825052799923));
#7364=CARTESIAN_POINT('Ctrl Pts',(96.1473323413611,1.65420923574938,-0.647777594852745));
#7365=CARTESIAN_POINT('Ctrl Pts',(96.1418649586059,1.62049403668184,-0.72964049025782));
#7366=CARTESIAN_POINT('Ctrl Pts',(96.1382788973759,1.59600569984257,-0.781755238240675));
#7367=CARTESIAN_POINT('Ctrl Pts',(96.1321223854516,1.55062686273318,-0.867272910072371));
#7368=CARTESIAN_POINT('Ctrl Pts',(96.1295932580675,1.53107714644833,-0.901336995056063));
#7369=CARTESIAN_POINT('Ctrl Pts',(96.1259182703506,1.50152186348764,-0.949095257506187));
#7370=CARTESIAN_POINT('Ctrl Pts',(96.1248052096535,1.49242344868247,-0.963338949442147));
#7371=CARTESIAN_POINT('Ctrl Pts',(96.1228444575935,1.47615074196743,-0.988030162692928));
#7372=CARTESIAN_POINT('Ctrl Pts',(96.1220001248121,1.46906521437369,-0.998534925310201));
#7373=CARTESIAN_POINT('Ctrl Pts',(96.1202349680317,1.45409463545272,-1.02022552892517));
#7374=CARTESIAN_POINT('Ctrl Pts',(96.1193134924493,1.44619150802514,-1.03139781005262));
#7375=CARTESIAN_POINT('Ctrl Pts',(96.11688640093,1.42515167703041,-1.06042352245404));
#7376=CARTESIAN_POINT('Ctrl Pts',(96.1153728865511,1.41180885801858,-1.07812384274513));
#7377=CARTESIAN_POINT('Ctrl Pts',(96.1075088181668,1.34137448488336,-1.16801048254654));
#7378=CARTESIAN_POINT('Ctrl Pts',(96.1009522451003,1.279074957092,-1.23591929776607));
#7379=CARTESIAN_POINT('Ctrl Pts',(96.0884369810071,1.15302173583489,-1.35353945693111));
#7380=CARTESIAN_POINT('Ctrl Pts',(96.0825238555979,1.0905834334467,-1.40433456704));
#7381=CARTESIAN_POINT('Ctrl Pts',(96.0736144279593,0.990465257690351,-1.47506688072342));
#7382=CARTESIAN_POINT('Ctrl Pts',(96.0705713942124,0.955151946663038,-1.49817519867346));
#7383=CARTESIAN_POINT('Ctrl Pts',(96.065696906075,0.896328910181318,-1.53374161948242));
#7384=CARTESIAN_POINT('Ctrl Pts',(96.0638352040829,0.873303959652029,-1.54696775906898));
#7385=CARTESIAN_POINT('Ctrl Pts',(96.0612966699708,0.841018065885381,-1.56456290114178));
#7386=CARTESIAN_POINT('Ctrl Pts',(96.06059553862,0.832004126180052,-1.56937490913489));
#7387=CARTESIAN_POINT('Ctrl Pts',(96.0594091779596,0.816577961339088,-1.57743975422904));
#7388=CARTESIAN_POINT('Ctrl Pts',(96.058921577677,0.810186688795131,-1.58073188182259));
#7389=CARTESIAN_POINT('Ctrl Pts',(96.057899317769,0.796676547085477,-1.5875874495117));
#7390=CARTESIAN_POINT('Ctrl Pts',(96.0573651942251,0.789553484107672,-1.59114195861709));
#7391=CARTESIAN_POINT('Ctrl Pts',(96.0559037556126,0.769895264690334,-1.60078716882656));
#7392=CARTESIAN_POINT('Ctrl Pts',(96.0549822893982,0.757311645158543,-1.60677857231766));
#7393=CARTESIAN_POINT('Ctrl Pts',(96.0493879199421,0.679856412915963,-1.64254498428812));
#7394=CARTESIAN_POINT('Ctrl Pts',(96.0449097627957,0.613301598140134,-1.66853898768166));
#7395=CARTESIAN_POINT('Ctrl Pts',(96.0336579349796,0.440269671422942,-1.72436047511622));
#7396=CARTESIAN_POINT('Ctrl Pts',(96.026980188727,0.332254115690725,-1.74838885050254));
#7397=CARTESIAN_POINT('Ctrl Pts',(96.0176297866786,0.184213907851702,-1.76709780608814));
#7398=CARTESIAN_POINT('Ctrl Pts',(96.0151732957584,0.145574176402628,-1.77069965970032));
#7399=CARTESIAN_POINT('Ctrl Pts',(96.0107803220572,0.0773083520507664,-1.77481360072315));
#7400=CARTESIAN_POINT('Ctrl Pts',(96.0088594725822,0.0477290226381277,-1.77585519562847));
#7401=CARTESIAN_POINT('Ctrl Pts',(96.0059174789471,0.00293958411527544,
-1.77631260239359));
#7402=CARTESIAN_POINT('Ctrl Pts',(96.0049132563282,-0.0122605817015053,
-1.77627271461423));
#7403=CARTESIAN_POINT('Ctrl Pts',(96.0031527711524,-0.0387417759068703,
-1.77586330888285));
#7404=CARTESIAN_POINT('Ctrl Pts',(96.0023992932645,-0.0500234251042128,
-1.77558133124439));
#7405=CARTESIAN_POINT('Ctrl Pts',(96.0006864631264,-0.0755461067529935,
-1.77469997516593));
#7406=CARTESIAN_POINT('Ctrl Pts',(95.9997251551623,-0.0897840005021764,
-1.7740366480704));
#7407=CARTESIAN_POINT('Ctrl Pts',(95.9971146343462,-0.128205631444982,-1.77178292225054));
#7408=CARTESIAN_POINT('Ctrl Pts',(95.9954554498375,-0.152366565774769,-1.76986884709633));
#7409=CARTESIAN_POINT('Ctrl Pts',(95.9837558204365,-0.320864485336603,-1.75304444636456));
#7410=CARTESIAN_POINT('Ctrl Pts',(95.9731652489588,-0.462913996172033,-1.72099202256592));
#7411=CARTESIAN_POINT('Ctrl Pts',(95.9583642421423,-0.653576288649097,-1.6526366980808));
#7412=CARTESIAN_POINT('Ctrl Pts',(95.9541785644385,-0.706729636315566,-1.63061461010219));
#7413=CARTESIAN_POINT('Ctrl Pts',(95.9477571517117,-0.78811212986688,-1.59216825771662));
#7414=CARTESIAN_POINT('Ctrl Pts',(95.9454662527019,-0.817116154218881,-1.57747963451054));
#7415=CARTESIAN_POINT('Ctrl Pts',(95.942456226926,-0.855376199582139,-1.55676479462481));
#7416=CARTESIAN_POINT('Ctrl Pts',(95.9417000568971,-0.865001097227207,-1.55143745795666));
#7417=CARTESIAN_POINT('Ctrl Pts',(95.9404489894633,-0.880957475654667,-1.54241101544268));
#7418=CARTESIAN_POINT('Ctrl Pts',(95.9399510829823,-0.887316556175685,-1.53876156400432));
#7419=CARTESIAN_POINT('Ctrl Pts',(95.9390010148878,-0.89947043673321,-1.53168609926305));
#7420=CARTESIAN_POINT('Ctrl Pts',(95.9385484399101,-0.905268613795681,-1.52826637531556));
#7421=CARTESIAN_POINT('Ctrl Pts',(95.9373165547804,-0.921069314523666,-1.5188257556306));
#7422=CARTESIAN_POINT('Ctrl Pts',(95.9365413793302,-0.931032353349821,-1.51273895080924));
#7423=CARTESIAN_POINT('Ctrl Pts',(95.9334386523684,-0.970953549639229,-1.48780572817097));
#7424=CARTESIAN_POINT('Ctrl Pts',(95.9311570894005,-1.00040743980018,-1.46816280606409));
#7425=CARTESIAN_POINT('Ctrl Pts',(95.9224343439896,-1.11235341354032,-1.38857101751339));
#7426=CARTESIAN_POINT('Ctrl Pts',(95.9162469296047,-1.19021507280611,-1.32244126257992));
#7427=CARTESIAN_POINT('Ctrl Pts',(95.9041191872546,-1.32897063129383,-1.18235524528025));
#7428=CARTESIAN_POINT('Ctrl Pts',(95.8982083459856,-1.39041099511642,-1.10945080248137));
#7429=CARTESIAN_POINT('Ctrl Pts',(95.8904394394053,-1.46029157284766,-1.01155444584408));
#7430=CARTESIAN_POINT('Ctrl Pts',(95.8888036478111,-1.47443693559598,-0.990822635789977));
#7431=CARTESIAN_POINT('Ctrl Pts',(95.8862100196735,-1.49594418338592,-0.957820177632319));
#7432=CARTESIAN_POINT('Ctrl Pts',(95.8852633972785,-1.50360544961536,-0.945747917912847));
#7433=CARTESIAN_POINT('Ctrl Pts',(95.8834767546907,-1.51770755677366,-0.922921950612268));
#7434=CARTESIAN_POINT('Ctrl Pts',(95.882638040963,-1.5241819614242,-0.912189941496587));
#7435=CARTESIAN_POINT('Ctrl Pts',(95.8807362186176,-1.53853226994615,-0.887823420743908));
#7436=CARTESIAN_POINT('Ctrl Pts',(95.8796707723648,-1.54634145138274,-0.874151050978877));
#7437=CARTESIAN_POINT('Ctrl Pts',(95.8763862728584,-1.56970698315513,-0.831949460391712));
#7438=CARTESIAN_POINT('Ctrl Pts',(95.8741463061002,-1.58466234777351,-0.803097080071995));
#7439=CARTESIAN_POINT('Ctrl Pts',(95.8623725387151,-1.65820214162449,-0.651160231893396));
#7440=CARTESIAN_POINT('Ctrl Pts',(95.8523915150334,-1.70325821519041,-0.52205705929633));
#7441=CARTESIAN_POINT('Ctrl Pts',(95.837086880413,-1.74916676237373,-0.317574761520012));
#7442=CARTESIAN_POINT('Ctrl Pts',(95.8317673133952,-1.76078359686751,-0.24511480604364));
#7443=CARTESIAN_POINT('Ctrl Pts',(95.8253774571049,-1.76961674749343,-0.154396793821098));
#7444=CARTESIAN_POINT('Ctrl Pts',(95.8241389160994,-1.7710771374349,-0.136629560796241));
#7445=CARTESIAN_POINT('Ctrl Pts',(95.8223121579015,-1.7728556718333,-0.110106707688259));
#7446=CARTESIAN_POINT('Ctrl Pts',(95.8217137503719,-1.77337688413802,-0.101366440216693));
#7447=CARTESIAN_POINT('Ctrl Pts',(95.8206871184338,-1.7741648731016,-0.0862754849370903));
#7448=CARTESIAN_POINT('Ctrl Pts',(95.8202572560546,-1.77446221688727,-0.0799268456068247));
#7449=CARTESIAN_POINT('Ctrl Pts',(95.8192500022411,-1.77508186827587,-0.0649803284838484));
#7450=CARTESIAN_POINT('Ctrl Pts',(95.818674183327,-1.77537579439365,-0.0563815445028544));
#7451=CARTESIAN_POINT('Ctrl Pts',(95.8169670492244,-1.77606581132273,-0.0307394339663348));
#7452=CARTESIAN_POINT('Ctrl Pts',(95.8158452404988,-1.7762790520397,-0.0136916335852668));
#7453=CARTESIAN_POINT('Ctrl Pts',(95.8058569137283,-1.77598936320795,0.139571542453031));
#7454=CARTESIAN_POINT('Ctrl Pts',(95.79767224834,-1.76006424360702,0.275323520346167));
#7455=CARTESIAN_POINT('Ctrl Pts',(95.7840093761035,-1.70914764296041,0.491100796826062));
#7456=CARTESIAN_POINT('Ctrl Pts',(95.7786838601724,-1.68354994538585,0.572732785812526));
#7457=CARTESIAN_POINT('Ctrl Pts',(95.7715022726718,-1.64268433392603,0.676255153691229));
#7458=CARTESIAN_POINT('Ctrl Pts',(95.7698179094051,-1.63266496171668,0.700098468406816));
#7459=CARTESIAN_POINT('Ctrl Pts',(95.7671647622894,-1.61623931686642,0.73691484913708));
#7460=CARTESIAN_POINT('Ctrl Pts',(95.7662080897019,-1.61018879729897,0.750043359101764));
#7461=CARTESIAN_POINT('Ctrl Pts',(95.7644126597065,-1.59860136190742,0.774399397664015));
#7462=CARTESIAN_POINT('Ctrl Pts',(95.7635753395328,-1.59310465495523,0.785645139936856));
#7463=CARTESIAN_POINT('Ctrl Pts',(95.7616902449042,-1.58052611485467,0.810704766537366));
#7464=CARTESIAN_POINT('Ctrl Pts',(95.7606403044382,-1.573381201103,0.824485650277882));
#7465=CARTESIAN_POINT('Ctrl Pts',(95.7579257106127,-1.55455862039561,0.859654176813744));
#7466=CARTESIAN_POINT('Ctrl Pts',(95.7562519639852,-1.54262012868615,0.880897748940143));
#7467=CARTESIAN_POINT('Ctrl Pts',(95.7464256325662,-1.47063969579265,1.00302817252497));
#7468=CARTESIAN_POINT('Ctrl Pts',(95.7379332657299,-1.40116005939237,1.09799289654791));
#7469=CARTESIAN_POINT('Ctrl Pts',(95.7239298355492,-1.27333678860947,1.24063663272306));
#7470=CARTESIAN_POINT('Ctrl Pts',(95.7184924732507,-1.22042260659681,1.29272403303986));
#7471=CARTESIAN_POINT('Ctrl Pts',(95.711340178858,-1.14506138807853,1.35814380783864));
#7472=CARTESIAN_POINT('Ctrl Pts',(95.7095199438121,-1.12535606069443,1.37451593606286));
#7473=CARTESIAN_POINT('Ctrl Pts',(95.7064181605257,-1.09076089563072,1.4020163373249));
#7474=CARTESIAN_POINT('Ctrl Pts',(95.7051262489749,-1.07603810565433,1.41334751736624));
#7475=CARTESIAN_POINT('Ctrl Pts',(95.7032370542885,-1.05400337544441,1.42976226444971));
#7476=CARTESIAN_POINT('Ctrl Pts',(95.7026285833451,-1.04682715687904,1.43502479437198));
#7477=CARTESIAN_POINT('Ctrl Pts',(95.7015442622734,-1.03389064340781,1.44436282875775));
#7478=CARTESIAN_POINT('Ctrl Pts',(95.7010671123727,-1.02814529912166,1.44845817757642));
#7479=CARTESIAN_POINT('Ctrl Pts',(95.6999988261138,-1.01516339262973,1.4575956674066));
#7480=CARTESIAN_POINT('Ctrl Pts',(95.6994089897435,-1.00791351863893,1.46261826550269));
#7481=CARTESIAN_POINT('Ctrl Pts',(95.6976150817076,-0.985623541884869,1.47781596155627));
#7482=CARTESIAN_POINT('Ctrl Pts',(95.6964220076421,-0.97046404878879,1.4878149667598));
#7483=CARTESIAN_POINT('Ctrl Pts',(95.6897493717963,-0.883968819634331,1.54298142280817));
#7484=CARTESIAN_POINT('Ctrl Pts',(95.6845216377863,-0.809629171838312,1.5832550317039));
#7485=CARTESIAN_POINT('Ctrl Pts',(95.674701715773,-0.664181357209329,1.64911624553048));
#7486=CARTESIAN_POINT('Ctrl Pts',(95.6701121242482,-0.593763265790631,1.67575837658732));
#7487=CARTESIAN_POINT('Ctrl Pts',(95.6610608490213,-0.454649415661084,1.71851783307174));
#7488=CARTESIAN_POINT('Ctrl Pts',(95.6566184865083,-0.386267692939748,1.73516720257875));
#7489=CARTESIAN_POINT('Ctrl Pts',(95.6507140889594,-0.296914735555921,1.75137828699455));
#7490=CARTESIAN_POINT('Ctrl Pts',(95.6493710514397,-0.276684058899716,1.75468804602519));
#7491=CARTESIAN_POINT('Ctrl Pts',(95.6471358948983,-0.243203130442738,1.75957216344348));
#7492=CARTESIAN_POINT('Ctrl Pts',(95.6462502105929,-0.229984009911182,1.76134871610423));
#7493=CARTESIAN_POINT('Ctrl Pts',(95.6445127132718,-0.204152872671202,1.76452448612535));
#7494=CARTESIAN_POINT('Ctrl Pts',(95.6436614005759,-0.191543373337164,1.76593776198209));
#7495=CARTESIAN_POINT('Ctrl Pts',(95.6416056159878,-0.161212996013897,1.76900853237707));
#7496=CARTESIAN_POINT('Ctrl Pts',(95.6403971044501,-0.143480542504504,1.77053497884845));
#7497=CARTESIAN_POINT('Ctrl Pts',(95.6362851695688,-0.0834944389435133,
1.77479166539372));
#7498=CARTESIAN_POINT('Ctrl Pts',(95.6333437714287,-0.0411698961341193,
1.77627736966851));
#7499=CARTESIAN_POINT('Ctrl Pts',(95.625696656016,0.0673416476502539,1.77620623763022));
#7500=CARTESIAN_POINT('Ctrl Pts',(95.620934451418,0.133458634067817,1.77246460935006));
#7501=CARTESIAN_POINT('Ctrl Pts',(95.6088790732658,0.298121982068145,1.75388030200898));
#7502=CARTESIAN_POINT('Ctrl Pts',(95.6015348677352,0.395923435846904,1.73442151491004));
#7503=CARTESIAN_POINT('Ctrl Pts',(95.5916229010142,0.528674836413008,1.69618898666391));
#7504=CARTESIAN_POINT('Ctrl Pts',(95.5888877211877,0.565413989852701,1.68429857096844));
#7505=CARTESIAN_POINT('Ctrl Pts',(95.585375856801,0.613056594757594,1.66714437314468));
#7506=CARTESIAN_POINT('Ctrl Pts',(95.5845473109883,0.624332631081921,1.66295445971391));
#7507=CARTESIAN_POINT('Ctrl Pts',(95.583209379177,0.642613237956164,1.65594965222455));
#7508=CARTESIAN_POINT('Ctrl Pts',(95.5826961133567,0.649643743825658,1.65320417245067));
#7509=CARTESIAN_POINT('Ctrl Pts',(95.5816828576435,0.663562120940664,1.64766641273418));
#7510=CARTESIAN_POINT('Ctrl Pts',(95.5811828068971,0.670450358746701,1.64487556267026));
#7511=CARTESIAN_POINT('Ctrl Pts',(95.5799160052794,0.687943434773452,1.63765989372201));
#7512=CARTESIAN_POINT('Ctrl Pts',(95.5791527521862,0.698523442117217,1.63317516363878));
#7513=CARTESIAN_POINT('Ctrl Pts',(95.5759615185912,0.742888354547811,1.61385943417819));
#7514=CARTESIAN_POINT('Ctrl Pts',(95.5735843700897,0.77625284968718,1.59807926411387));
#7515=CARTESIAN_POINT('Ctrl Pts',(95.5667343953338,0.87237081149124,1.54889763119721));
#7516=CARTESIAN_POINT('Ctrl Pts',(95.5623638008931,0.93364212962893,1.51275525330887));
#7517=CARTESIAN_POINT('Ctrl Pts',(95.5505174098619,1.0936450894637,1.40493933661967));
#7518=CARTESIAN_POINT('Ctrl Pts',(95.5430649397026,1.18741679163067,1.32663164266866));
#7519=CARTESIAN_POINT('Ctrl Pts',(95.5336515557619,1.28933674948063,1.22199093018612));
#7520=CARTESIAN_POINT('Ctrl Pts',(95.5320765746302,1.30588424271542,1.20429121942383));
#7521=CARTESIAN_POINT('Ctrl Pts',(95.5294701966113,1.33240388976126,1.17473556481106));
#7522=CARTESIAN_POINT('Ctrl Pts',(95.5284479057122,1.34259245340436,1.1630774915711));
#7523=CARTESIAN_POINT('Ctrl Pts',(95.526587794063,1.36073848934771,1.14175804873563));
#7524=CARTESIAN_POINT('Ctrl Pts',(95.5257522245866,1.36874879658817,1.13214283387398));
#7525=CARTESIAN_POINT('Ctrl Pts',(95.5239404345869,1.38581048569498,1.1112169897048));
#7526=CARTESIAN_POINT('Ctrl Pts',(95.5229628642119,1.39482638505668,1.09987873619199));
#7527=CARTESIAN_POINT('Ctrl Pts',(95.5202144155178,1.41963978328277,1.06787799251214));
#7528=CARTESIAN_POINT('Ctrl Pts',(95.5184314249069,1.43512305180507,1.04697766091598));
#7529=CARTESIAN_POINT('Ctrl Pts',(95.5106396972869,1.5001219296749,0.955085942278702));
#7530=CARTESIAN_POINT('Ctrl Pts',(95.50445891989,1.54486432781,0.880877595526095));
#7531=CARTESIAN_POINT('Ctrl Pts',(95.4884237680268,1.64476288353193,0.683990516287231));
#7532=CARTESIAN_POINT('Ctrl Pts',(95.4784520596189,1.69174164374578,0.557764116329369));
#7533=CARTESIAN_POINT('Ctrl Pts',(95.467823869387,1.72824699052075,0.410524503161078));
#7534=CARTESIAN_POINT('Ctrl Pts',(95.4666130685231,1.73219337590142,0.393540586785368));
#7535=CARTESIAN_POINT('Ctrl Pts',(95.4648188803351,1.73772898071901,0.368018188507811));
#7536=CARTESIAN_POINT('Ctrl Pts',(95.4642258051852,1.7395065866799,0.359522239049211));
#7537=CARTESIAN_POINT('Ctrl Pts',(95.4632047610572,1.74247720472665,0.344786318748178));
#7538=CARTESIAN_POINT('Ctrl Pts',(95.4627752137472,1.74369909258552,0.338552643482281));
#7539=CARTESIAN_POINT('Ctrl Pts',(95.4617635255774,1.74651068104241,0.323789702221176));
#7540=CARTESIAN_POINT('Ctrl Pts',(95.4611830171794,1.74807136764266,0.315255185170671));
#7541=CARTESIAN_POINT('Ctrl Pts',(95.459447129513,1.75257655302122,0.28955614842903));
#7542=CARTESIAN_POINT('Ctrl Pts',(95.4583017389889,1.75533132109198,0.272358855766785));
#7543=CARTESIAN_POINT('Ctrl Pts',(95.4526382998094,1.76782129619378,0.18630121235037));
#7544=CARTESIAN_POINT('Ctrl Pts',(95.448290181176,1.7737605212833,0.116944363334072));
#7545=CARTESIAN_POINT('Ctrl Pts',(95.4420352323939,1.77646257458917,0.0157485988176179));
#7546=CARTESIAN_POINT('Ctrl Pts',(95.440091044771,1.77646049673819,-0.0159138844807851));
#7547=CARTESIAN_POINT('Ctrl Pts',(95.4381488292622,1.77561363320029,-0.0475424872432087));
#7548=CARTESIAN_POINT('',(95.4827176862982,0.000795599009507856,1.77624982182187));
#7549=CARTESIAN_POINT('Ctrl Pts',(95.2889037169497,1.77561363837295,-0.0475422940546111));
#7550=CARTESIAN_POINT('Ctrl Pts',(95.2897480647306,1.77595726937842,-0.0347083340615077));
#7551=CARTESIAN_POINT('Ctrl Pts',(95.2905966195916,1.77616174091978,-0.0218712350535019));
#7552=CARTESIAN_POINT('Ctrl Pts',(95.2922811358752,1.77629068903477,0.00348412783102648));
#7553=CARTESIAN_POINT('Ctrl Pts',(95.2931168284974,1.77622202669782,0.0160015365959801));
#7554=CARTESIAN_POINT('Ctrl Pts',(95.2949259376486,1.77578916117662,0.0429602236757479));
#7555=CARTESIAN_POINT('Ctrl Pts',(95.2959006712007,1.77538107689167,0.0573997916003285));
#7556=CARTESIAN_POINT('Ctrl Pts',(95.2986327151757,1.77375307414394,0.0976236153042587));
#7557=CARTESIAN_POINT('Ctrl Pts',(95.3004019048997,1.77214719495702,0.123387744904151));
#7558=CARTESIAN_POINT('Ctrl Pts',(95.3080774447668,1.76283725475589,0.233902057791716));
#7559=CARTESIAN_POINT('Ctrl Pts',(95.314149796804,1.74961077559695,0.318062621267385));
#7560=CARTESIAN_POINT('Ctrl Pts',(95.3299315432877,1.70053412170142,0.529870729698813));
#7561=CARTESIAN_POINT('Ctrl Pts',(95.3397599148447,1.65634522364526,0.655058599028514));
#7562=CARTESIAN_POINT('Ctrl Pts',(95.3504614292562,1.59001249145733,0.792034045329869));
#7563=CARTESIAN_POINT('Ctrl Pts',(95.3518432033154,1.58106662819951,0.809744435590271));
#7564=CARTESIAN_POINT('Ctrl Pts',(95.3538368460025,1.56757243095919,0.835382618322914));
#7565=CARTESIAN_POINT('Ctrl Pts',(95.3544616728043,1.56325703680746,0.843430430661255));
#7566=CARTESIAN_POINT('Ctrl Pts',(95.3555629191811,1.55549423342535,0.857643067696634));
#7567=CARTESIAN_POINT('Ctrl Pts',(95.3560408308539,1.5520718858252,0.863821051232642));
#7568=CARTESIAN_POINT('Ctrl Pts',(95.3570961488097,1.5443952464054,0.877485913187523));
#7569=CARTESIAN_POINT('Ctrl Pts',(95.357672430337,1.5401232699767,0.884962443250514));
#7570=CARTESIAN_POINT('Ctrl Pts',(95.3593824543972,1.52721352768129,0.907179576641817));
#7571=CARTESIAN_POINT('Ctrl Pts',(95.3605066421698,1.51841700988203,0.921827413578864));
#7572=CARTESIAN_POINT('Ctrl Pts',(95.3659622732344,1.47428508204245,0.992968987845695));
#7573=CARTESIAN_POINT('Ctrl Pts',(95.370137405077,1.43599784132198,1.04757625256597));
#7574=CARTESIAN_POINT('Ctrl Pts',(95.3837818726047,1.29944008789964,1.22073713171126));
#7575=CARTESIAN_POINT('Ctrl Pts',(95.3930287272009,1.18886389514128,1.32866254075628));
#7576=CARTESIAN_POINT('Ctrl Pts',(95.4044901795697,1.04664671799196,1.43532777786403));
#7577=CARTESIAN_POINT('Ctrl Pts',(95.4060442387585,1.02724172054587,1.44927897340892));
#7578=CARTESIAN_POINT('Ctrl Pts',(95.4086231816926,0.994890756746498,1.47156147415257));
#7579=CARTESIAN_POINT('Ctrl Pts',(95.4096392927381,0.982107110040264,1.48012377509035));
#7580=CARTESIAN_POINT('Ctrl Pts',(95.4114928873141,0.958731703293867,1.49534412498387));
#7581=CARTESIAN_POINT('Ctrl Pts',(95.4123281944281,0.948177662924896,1.50205846649818));
#7582=CARTESIAN_POINT('Ctrl Pts',(95.4141448510894,0.925187221370135,1.51634582557369));
#7583=CARTESIAN_POINT('Ctrl Pts',(95.415127611126,0.912726934048016,1.52387846600492));
#7584=CARTESIAN_POINT('Ctrl Pts',(95.4179064750809,0.877439345272682,1.54462288368058));
#7585=CARTESIAN_POINT('Ctrl Pts',(95.4197151303545,0.854409181742743,1.55748016918706));
#7586=CARTESIAN_POINT('Ctrl Pts',(95.4277273623025,0.752165852048041,1.61161039089555));
#7587=CARTESIAN_POINT('Ctrl Pts',(95.4341147851219,0.67020116420117,1.64738209155729));
#7588=CARTESIAN_POINT('Ctrl Pts',(95.4471648173014,0.500755366929287,1.70658837214136));
#7589=CARTESIAN_POINT('Ctrl Pts',(95.4538102893005,0.413463621563228,1.72981145364995));
#7590=CARTESIAN_POINT('Ctrl Pts',(95.4638215852848,0.277182520490236,1.75515764743322));
#7591=CARTESIAN_POINT('Ctrl Pts',(95.4672749072743,0.229232446356009,1.7620618286026));
#7592=CARTESIAN_POINT('Ctrl Pts',(95.471534092154,0.168252665807003,1.76831013935905));
#7593=CARTESIAN_POINT('Ctrl Pts',(95.4724219609697,0.155434993547325,1.76948288930693));
#7594=CARTESIAN_POINT('Ctrl Pts',(95.4738313781281,0.134900281988557,1.77113684621543));
#7595=CARTESIAN_POINT('Ctrl Pts',(95.4743575720501,0.127191162104832,1.7717071507879));
#7596=CARTESIAN_POINT('Ctrl Pts',(95.4753331304126,0.112814139200693,1.77267640771399));
#7597=CARTESIAN_POINT('Ctrl Pts',(95.4757831760955,0.106147377196289,1.77308810060367));
#7598=CARTESIAN_POINT('Ctrl Pts',(95.4767200729813,0.0922005598590766,1.77387041588002));
#7599=CARTESIAN_POINT('Ctrl Pts',(95.4772065323742,0.0849201555293663,1.77423385362435));
#7600=CARTESIAN_POINT('Ctrl Pts',(95.4784450815012,0.0662910261649312,1.77504888740892));
#7601=CARTESIAN_POINT('Ctrl Pts',(95.4791938865745,0.0549396407647299,1.77543648280939));
#7602=CARTESIAN_POINT('Ctrl Pts',(95.4808718906935,0.0293249217568935,1.77606519674254));
#7603=CARTESIAN_POINT('Ctrl Pts',(95.4817981529735,0.0150607598054103,1.77624343232211));
#7604=CARTESIAN_POINT('Ctrl Pts',(95.4827176862982,0.000795599009507856,
1.77624982182187));
#7605=CARTESIAN_POINT('Ctrl Pts',(95.4827175421507,0.000797835238689031,
1.77624982081883));
#7606=CARTESIAN_POINT('Ctrl Pts',(95.4904658484486,-0.119405257906508,1.77630381224638));
#7607=CARTESIAN_POINT('Ctrl Pts',(95.4977298043407,-0.239323346943683,1.76415612306193));
#7608=CARTESIAN_POINT('Ctrl Pts',(95.5091636269205,-0.421325828350258,1.72680218931832));
#7609=CARTESIAN_POINT('Ctrl Pts',(95.5132254239558,-0.484757860705407,1.71007899243386));
#7610=CARTESIAN_POINT('Ctrl Pts',(95.5192359260755,-0.574970268013196,1.68087190865953));
#7611=CARTESIAN_POINT('Ctrl Pts',(95.5211088640415,-0.602595015656902,1.67116734277415));
#7612=CARTESIAN_POINT('Ctrl Pts',(95.5245490858155,-0.652314864208148,1.65230769089842));
#7613=CARTESIAN_POINT('Ctrl Pts',(95.5261090025806,-0.67448918367119,1.64338055235981));
#7614=CARTESIAN_POINT('Ctrl Pts',(95.5286095683612,-0.709399870739571,1.62850031125412));
#7615=CARTESIAN_POINT('Ctrl Pts',(95.5295403438087,-0.722257813532284,1.62283858470574));
#7616=CARTESIAN_POINT('Ctrl Pts',(95.5313140225818,-0.746492458131851,1.61182230444266));
#7617=CARTESIAN_POINT('Ctrl Pts',(95.5321558318,-0.757882154425968,1.60649829041125));
#7618=CARTESIAN_POINT('Ctrl Pts',(95.5340885011393,-0.783769149252214,1.59406108160048));
#7619=CARTESIAN_POINT('Ctrl Pts',(95.5351820099695,-0.798227703459158,1.58687028913103));
#7620=CARTESIAN_POINT('Ctrl Pts',(95.5386505529621,-0.843485118623139,1.56358702511387));
#7621=CARTESIAN_POINT('Ctrl Pts',(95.5410500675465,-0.873909275212359,1.54678822577836));
#7622=CARTESIAN_POINT('Ctrl Pts',(95.5528356447427,-1.01902314148532,1.46101491836367));
#7623=CARTESIAN_POINT('Ctrl Pts',(95.5626410462503,-1.12614720049667,1.38012838302095));
#7624=CARTESIAN_POINT('Ctrl Pts',(95.5777033090374,-1.27573075314451,1.23807589445349));
#7625=CARTESIAN_POINT('Ctrl Pts',(95.5829623415775,-1.32520412097489,1.18497127545016));
#7626=CARTESIAN_POINT('Ctrl Pts',(95.5892889151992,-1.38257129010113,1.11529160147115));
#7627=CARTESIAN_POINT('Ctrl Pts',(95.59052131656,-1.393640873137,1.1014281207151));
#7628=CARTESIAN_POINT('Ctrl Pts',(95.5923408599228,-1.40985105737297,1.08049082394988));
#7629=CARTESIAN_POINT('Ctrl Pts',(95.5929380802453,-1.41514977619948,1.07354158916254));
#7630=CARTESIAN_POINT('Ctrl Pts',(95.593963448654,-1.42421275628829,1.0614718404399));
#7631=CARTESIAN_POINT('Ctrl Pts',(95.5943932215669,-1.42800104920147,1.05636994003308));
#7632=CARTESIAN_POINT('Ctrl Pts',(95.595401375667,-1.43686282777616,1.04430051022357));
#7633=CARTESIAN_POINT('Ctrl Pts',(95.595978171669,-1.44191308033597,1.03731625746418));
#7634=CARTESIAN_POINT('Ctrl Pts',(95.5976913401766,-1.45684541072503,1.01634579049538));
#7635=CARTESIAN_POINT('Ctrl Pts',(95.5988181056185,-1.46657659785096,1.0022526889506));
#7636=CARTESIAN_POINT('Ctrl Pts',(95.6071188494788,-1.53743412762817,0.896391513343246));
#7637=CARTESIAN_POINT('Ctrl Pts',(95.613847156059,-1.59010891703738,0.799238145194436));
#7638=CARTESIAN_POINT('Ctrl Pts',(95.6254375979447,-1.66428917893848,0.625597948211356));
#7639=CARTESIAN_POINT('Ctrl Pts',(95.6302645246951,-1.69031630186238,0.551417209256785));
#7640=CARTESIAN_POINT('Ctrl Pts',(95.6382498467306,-1.7242052599363,0.429516284835134));
#7641=CARTESIAN_POINT('Ctrl Pts',(95.6413229183178,-1.73518096171951,0.382772023256816));
#7642=CARTESIAN_POINT('Ctrl Pts',(95.6456415182285,-1.74768269828848,0.317803856105381));
#7643=CARTESIAN_POINT('Ctrl Pts',(95.6468355615283,-1.75084157994094,0.299913031651014));
#7644=CARTESIAN_POINT('Ctrl Pts',(95.6488910804261,-1.7557701744631,0.269260219130472));
#7645=CARTESIAN_POINT('Ctrl Pts',(95.6497481709408,-1.75767650890935,0.256521434276438));
#7646=CARTESIAN_POINT('Ctrl Pts',(95.6513925762957,-1.76105040700204,0.232169185724215));
#7647=CARTESIAN_POINT('Ctrl Pts',(95.6521790809028,-1.76254204876103,0.220559701103775));
#7648=CARTESIAN_POINT('Ctrl Pts',(95.6540361131477,-1.76577774886916,0.193242737959454));
#7649=CARTESIAN_POINT('Ctrl Pts',(95.6551095624317,-1.76742710328808,0.177525267253876));
#7650=CARTESIAN_POINT('Ctrl Pts',(95.6589383313237,-1.77252977756963,0.121736630974516));
#7651=CARTESIAN_POINT('Ctrl Pts',(95.6617289029506,-1.77483144840728,0.08157511874713));
#7652=CARTESIAN_POINT('Ctrl Pts',(95.6735074028595,-1.77873129869303,-0.0858111367228625));
#7653=CARTESIAN_POINT('Ctrl Pts',(95.6828433037144,-1.76802159381666,-0.212931268975042));
#7654=CARTESIAN_POINT('Ctrl Pts',(95.6959240255116,-1.73393592621098,-0.388895171229194));
#7655=CARTESIAN_POINT('Ctrl Pts',(95.6997021873171,-1.72179549789788,-0.439538585422724));
#7656=CARTESIAN_POINT('Ctrl Pts',(95.7048925824717,-1.7017050882026,-0.509605655292844));
#7657=CARTESIAN_POINT('Ctrl Pts',(95.7063642489638,-1.6956104469003,-0.529531324781816));
#7658=CARTESIAN_POINT('Ctrl Pts',(95.7089314794952,-1.68424906163052,-0.564466080873819));
#7659=CARTESIAN_POINT('Ctrl Pts',(95.7100334310342,-1.67912875316064,-0.579520087998707));
#7660=CARTESIAN_POINT('Ctrl Pts',(95.7116990281738,-1.67100460468127,-0.602393367067877));
#7661=CARTESIAN_POINT('Ctrl Pts',(95.7122704957538,-1.66814661846772,-0.610263077739285));
#7662=CARTESIAN_POINT('Ctrl Pts',(95.7133196219961,-1.66276684639011,-0.624756514314161));
#7663=CARTESIAN_POINT('Ctrl Pts',(95.7137981320778,-1.66026100605841,-0.631385525644804));
#7664=CARTESIAN_POINT('Ctrl Pts',(95.7148985779523,-1.65437821466577,-0.646670789129523));
#7665=CARTESIAN_POINT('Ctrl Pts',(95.715518837265,-1.65097293702323,-0.655315769244813));
#7666=CARTESIAN_POINT('Ctrl Pts',(95.7175495539603,-1.63953441918701,-0.683699555264158));
#7667=CARTESIAN_POINT('Ctrl Pts',(95.7189441693934,-1.63121345768394,-0.703321368262269));
#7668=CARTESIAN_POINT('Ctrl Pts',(95.7277137753823,-1.576062593838,-0.827125750951435));
#7669=CARTESIAN_POINT('Ctrl Pts',(95.7346475210422,-1.51962304985306,-0.92674831504206));
#7670=CARTESIAN_POINT('Ctrl Pts',(95.7479492671776,-1.39526052170655,-1.10397905822821));
#7671=CARTESIAN_POINT('Ctrl Pts',(95.7542768642277,-1.32940943107528,-1.18245032989773));
#7672=CARTESIAN_POINT('Ctrl Pts',(95.7625026112235,-1.23944150553618,-1.27258761341929));
#7673=CARTESIAN_POINT('Ctrl Pts',(95.7641391680124,-1.22133005931005,-1.28997955935986));
#7674=CARTESIAN_POINT('Ctrl Pts',(95.7667337122914,-1.19233466205341,-1.31666495661527));
#7675=CARTESIAN_POINT('Ctrl Pts',(95.767680471494,-1.18169625332925,-1.32622113504322));
#7676=CARTESIAN_POINT('Ctrl Pts',(95.7694671940761,-1.1615198335759,-1.34390952480264));
#7677=CARTESIAN_POINT('Ctrl Pts',(95.7703058488285,-1.15200882540806,-1.35207129505764));
#7678=CARTESIAN_POINT('Ctrl Pts',(95.7722072941982,-1.13035942582877,-1.3702552299091));
#7679=CARTESIAN_POINT('Ctrl Pts',(95.77327241917,-1.1181727166752,-1.38021794455292));
#7680=CARTESIAN_POINT('Ctrl Pts',(95.7765549810348,-1.08044547891101,-1.41023259322138));
#7681=CARTESIAN_POINT('Ctrl Pts',(95.7787932961479,-1.05448743003822,-1.42974627789123));
#7682=CARTESIAN_POINT('Ctrl Pts',(95.7905669729014,-0.916829452409413,-1.52744064427992));
#7683=CARTESIAN_POINT('Ctrl Pts',(95.800549853815,-0.796948921754993,-1.59327075624083));
#7684=CARTESIAN_POINT('Ctrl Pts',(95.8158570789823,-0.602860632897499,-1.6724229264151));
#7685=CARTESIAN_POINT('Ctrl Pts',(95.8211773104897,-0.533316541880481,-1.69588174868033));
#7686=CARTESIAN_POINT('Ctrl Pts',(95.8275678407284,-0.445304538327723,-1.71961789223093));
#7687=CARTESIAN_POINT('Ctrl Pts',(95.8288064299105,-0.428023776423409,-1.72400044507977));
#7688=CARTESIAN_POINT('Ctrl Pts',(95.8306332314175,-0.40216101172052,-1.73014659489159));
#7689=CARTESIAN_POINT('Ctrl Pts',(95.8312316351064,-0.393627781506541,-1.73210793455745));
#7690=CARTESIAN_POINT('Ctrl Pts',(95.8322582480551,-0.378875940428328,-1.73538395610821));
#7691=CARTESIAN_POINT('Ctrl Pts',(95.832688095378,-0.372664411742228,-1.73672844542116));
#7692=CARTESIAN_POINT('Ctrl Pts',(95.8336952933583,-0.358027683410053,-1.73981442961415));
#7693=CARTESIAN_POINT('Ctrl Pts',(95.8342710718519,-0.349596891582212,-1.74152809127037));
#7694=CARTESIAN_POINT('Ctrl Pts',(95.8359780244609,-0.324425785132821,-1.7464542694911));
#7695=CARTESIAN_POINT('Ctrl Pts',(95.8370996947708,-0.307650789276348,-1.74948725343086));
#7696=CARTESIAN_POINT('Ctrl Pts',(95.8470885985108,-0.156447583644824,-1.77458316863787));
#7697=CARTESIAN_POINT('Ctrl Pts',(95.8552738483938,-0.019922168732767,-1.78135766408638));
#7698=CARTESIAN_POINT('Ctrl Pts',(95.8689370723993,0.201312685185786,-1.76687237439998));
#7699=CARTESIAN_POINT('Ctrl Pts',(95.8742622882672,0.286051313500328,-1.75514587297028));
#7700=CARTESIAN_POINT('Ctrl Pts',(95.8814434860663,0.394905414453724,-1.73198802296109));
#7701=CARTESIAN_POINT('Ctrl Pts',(95.8831277808173,0.420077630275489,-1.72605546592914));
#7702=CARTESIAN_POINT('Ctrl Pts',(95.8857808221302,0.459104114651419,-1.71595350175356));
#7703=CARTESIAN_POINT('Ctrl Pts',(95.8867374584725,0.473052763193094,-1.71216064395958));
#7704=CARTESIAN_POINT('Ctrl Pts',(95.8885328206763,0.498990362079987,-1.70476665505639));
#7705=CARTESIAN_POINT('Ctrl Pts',(95.8893701094222,0.510990615446308,-1.70120819029301));
#7706=CARTESIAN_POINT('Ctrl Pts',(95.8912551325656,0.537786188428529,-1.69295334120882));
#7707=CARTESIAN_POINT('Ctrl Pts',(95.8923050328096,0.552559410563726,-1.68818928768357));
#7708=CARTESIAN_POINT('Ctrl Pts',(95.8950195178779,0.59035782903476,-1.67545080313108));
#7709=CARTESIAN_POINT('Ctrl Pts',(95.8966931952179,0.613284143432193,-1.66719531459211));
#7710=CARTESIAN_POINT('Ctrl Pts',(95.9065212778656,0.745671858290243,-1.61642392883029));
#7711=CARTESIAN_POINT('Ctrl Pts',(95.915015636956,0.850853664247691,-1.5636150925841));
#7712=CARTESIAN_POINT('Ctrl Pts',(95.9290197240891,1.0126978104176,-1.46116608767325));
#7713=CARTESIAN_POINT('Ctrl Pts',(95.9344557472441,1.07281273015068,-1.41761665117643));
#7714=CARTESIAN_POINT('Ctrl Pts',(95.9416064787261,1.14979144342763,-1.35414166147278));
#7715=CARTESIAN_POINT('Ctrl Pts',(95.9434264528082,1.16919777194216,-1.3374216647518));
#7716=CARTESIAN_POINT('Ctrl Pts',(95.9465278324851,1.20204290686763,-1.30786158116165));
#7717=CARTESIAN_POINT('Ctrl Pts',(95.947819598296,1.21565409917173,-1.29521976694221));
#7718=CARTESIAN_POINT('Ctrl Pts',(95.9497086095095,1.23548909754919,-1.27620920220812));
#7719=CARTESIAN_POINT('Ctrl Pts',(95.9503170400925,1.24186688338772,-1.27000389387438));
#7720=CARTESIAN_POINT('Ctrl Pts',(95.9514013025132,1.25321758366416,-1.25879288518818));
#7721=CARTESIAN_POINT('Ctrl Pts',(95.9518784338275,1.25820758891953,-1.25380521121105));
#7722=CARTESIAN_POINT('Ctrl Pts',(95.9529466919265,1.26936835079225,-1.24251592781981));
#7723=CARTESIAN_POINT('Ctrl Pts',(95.9535365186582,1.27552203786981,-1.23619795342259));
#7724=CARTESIAN_POINT('Ctrl Pts',(95.9553304348032,1.294201073173,-1.21673225259117));
#7725=CARTESIAN_POINT('Ctrl Pts',(95.9565235260953,1.30657252251288,-1.20343761719195));
#7726=CARTESIAN_POINT('Ctrl Pts',(95.9632017706111,1.37535814647265,-1.12720763185612));
#7727=CARTESIAN_POINT('Ctrl Pts',(95.9684345601213,1.42743415394807,-1.0604914742689));
#7728=CARTESIAN_POINT('Ctrl Pts',(95.9782650772373,1.5165495807386,-0.927799566828433));
#7729=CARTESIAN_POINT('Ctrl Pts',(95.9828601390191,1.55451526920906,-0.862679909605681));
#7730=CARTESIAN_POINT('Ctrl Pts',(95.9904587312238,1.60921892190076,-0.753442197148421));
#7731=CARTESIAN_POINT('Ctrl Pts',(95.9934041099408,1.62853689295622,-0.710723439367341));
#7732=CARTESIAN_POINT('Ctrl Pts',(95.9985728161762,1.65891227367051,-0.635790536255283));
#7733=CARTESIAN_POINT('Ctrl Pts',(96.0007710000303,1.67077467838041,-0.603929855632468));
#7734=CARTESIAN_POINT('Ctrl Pts',(96.0040490325652,1.68687006018066,-0.556587756553879));
#7735=CARTESIAN_POINT('Ctrl Pts',(96.0051053581694,1.69181950793591,-0.54135686501542));
#7736=CARTESIAN_POINT('Ctrl Pts',(96.007002159096,1.70028153635546,-0.514066602218984));
#7737=CARTESIAN_POINT('Ctrl Pts',(96.0078399699372,1.70387346810471,-0.502032832754761));
#7738=CARTESIAN_POINT('Ctrl Pts',(96.0096291565387,1.71123401666494,-0.476384040351836));
#7739=CARTESIAN_POINT('Ctrl Pts',(96.0105815824227,1.71496839714795,-0.462760186676333));
#7740=CARTESIAN_POINT('Ctrl Pts',(96.013184972328,1.72467647158157,-0.425610440871128));
#7741=CARTESIAN_POINT('Ctrl Pts',(96.0148460540379,1.73033089524674,-0.402005062453215));
#7742=CARTESIAN_POINT('Ctrl Pts',(96.0242162553543,1.75922401354049,-0.269451460646902));
#7743=CARTESIAN_POINT('Ctrl Pts',(96.0322271973074,1.77263710159839,-0.158710346315969));
#7744=CARTESIAN_POINT('Ctrl Pts',(96.0403469459233,1.77561363956144,-0.0475422496666396));
#7745=CARTESIAN_POINT('Origin',(88.3562164250559,0.,0.));
#7746=CARTESIAN_POINT('',(96.9396785508644,1.77561363580749,-0.0475423898693833));
#7747=CARTESIAN_POINT('',(96.7921246218182,1.77561363837209,-0.0475422940869062));
#7748=CARTESIAN_POINT('',(88.3562164250559,1.77561363837197,-0.0475422940912398));
#7749=CARTESIAN_POINT('',(96.3799606556061,-0.00136080493914694,1.776249478736));
#7750=CARTESIAN_POINT('Ctrl Pts',(96.9396785508644,1.77561363580749,-0.0475423898693833));
#7751=CARTESIAN_POINT('Ctrl Pts',(96.9360093059474,1.77422561861672,-0.0993820693100051));
#7752=CARTESIAN_POINT('Ctrl Pts',(96.9322809403556,1.77056776805062,-0.151147512117908));
#7753=CARTESIAN_POINT('Ctrl Pts',(96.9191246470724,1.74988061234432,-0.331252339869889));
#7754=CARTESIAN_POINT('Ctrl Pts',(96.9095195712726,1.72110911674852,-0.45781568684712));
#7755=CARTESIAN_POINT('Ctrl Pts',(96.8988544704244,1.671736746555,-0.600694276812251));
#7756=CARTESIAN_POINT('Ctrl Pts',(96.897334790537,1.66425372143838,-0.621125606865727));
#7757=CARTESIAN_POINT('Ctrl Pts',(96.895227241329,1.65321617704534,-0.649629059745425));
#7758=CARTESIAN_POINT('Ctrl Pts',(96.8946231374856,1.64997441799014,-0.657819178349955));
#7759=CARTESIAN_POINT('Ctrl Pts',(96.8935342771295,1.64398687160514,-0.672623600189202));
#7760=CARTESIAN_POINT('Ctrl Pts',(96.8930483437481,1.6412617559151,-0.67924605086048));
#7761=CARTESIAN_POINT('Ctrl Pts',(96.8920361001067,1.63547226459627,-0.693077110426369));
#7762=CARTESIAN_POINT('Ctrl Pts',(96.8915102539116,1.6324001547973,-0.700282192993025));
#7763=CARTESIAN_POINT('Ctrl Pts',(96.890096070414,1.62396631454137,-0.719705138247724));
#7764=CARTESIAN_POINT('Ctrl Pts',(96.8892129699055,1.61851429843332,-0.731883576115109));
#7765=CARTESIAN_POINT('Ctrl Pts',(96.8842364908465,1.58676778662181,-0.800707182560501));
#7766=CARTESIAN_POINT('Ctrl Pts',(96.8802924573034,1.55763475141609,-0.856002179490291));
#7767=CARTESIAN_POINT('Ctrl Pts',(96.8713938245461,1.48434481681995,-0.978922127165139));
#7768=CARTESIAN_POINT('Ctrl Pts',(96.8664872959909,1.43837325200844,-1.04529953297451));
#7769=CARTESIAN_POINT('Ctrl Pts',(96.8558670927954,1.33086218804632,-1.17994479194519));
#7770=CARTESIAN_POINT('Ctrl Pts',(96.8501474548075,1.26822487890994,-1.24702305268568));
#7771=CARTESIAN_POINT('Ctrl Pts',(96.8427676440197,1.18436965890199,-1.32394240395596));
#7772=CARTESIAN_POINT('Ctrl Pts',(96.8413188746332,1.16776369362043,-1.33861228981251));
#7773=CARTESIAN_POINT('Ctrl Pts',(96.8389545435269,1.1404658331325,-1.36183294649985));
#7774=CARTESIAN_POINT('Ctrl Pts',(96.8380470216527,1.12994156612425,-1.37057773589062));
#7775=CARTESIAN_POINT('Ctrl Pts',(96.8362894626513,1.10947850720572,-1.3871849455467));
#7776=CARTESIAN_POINT('Ctrl Pts',(96.8354401849797,1.09955451380068,-1.39506433108703));
#7777=CARTESIAN_POINT('Ctrl Pts',(96.8334478251796,1.07619578153063,-1.41320645946733));
#7778=CARTESIAN_POINT('Ctrl Pts',(96.8323015038403,1.06269733787398,-1.4233847655494));
#7779=CARTESIAN_POINT('Ctrl Pts',(96.8284654965265,1.01734732216772,-1.45657560758094));
#7780=CARTESIAN_POINT('Ctrl Pts',(96.8257433391813,0.984879592647276,-1.4787223679309));
#7781=CARTESIAN_POINT('Ctrl Pts',(96.8189383221161,0.903064194746767,-1.53063971570956));
#7782=CARTESIAN_POINT('Ctrl Pts',(96.8148159662628,0.852953441844098,-1.55911905917351));
#7783=CARTESIAN_POINT('Ctrl Pts',(96.8084876862627,0.774972299625833,-1.59855219210809));
#7784=CARTESIAN_POINT('Ctrl Pts',(96.8063189488297,0.748059638292484,-1.6113217790696));
#7785=CARTESIAN_POINT('Ctrl Pts',(96.7958527604181,0.617045506082863,-1.66949576013225));
#7786=CARTESIAN_POINT('Ctrl Pts',(96.7874807863699,0.509064051667179,-1.70552597484869));
#7787=CARTESIAN_POINT('Ctrl Pts',(96.7783594449398,0.382084610481223,-1.73474921692463));
#7788=CARTESIAN_POINT('Ctrl Pts',(96.7771991858427,0.365741355284067,-1.73826833565245));
#7789=CARTESIAN_POINT('Ctrl Pts',(96.7754570551955,0.340875220570857,-1.74325639560033));
#7790=CARTESIAN_POINT('Ctrl Pts',(96.7748664987088,0.332387784988062,-1.74489459425764));
#7791=CARTESIAN_POINT('Ctrl Pts',(96.7738478964405,0.317641325929384,-1.74762937149171));
#7792=CARTESIAN_POINT('Ctrl Pts',(96.7734183021193,0.311388056323577,-1.7487543891584));
#7793=CARTESIAN_POINT('Ctrl Pts',(96.7724041406368,0.296545448095909,-1.75134256200132));
#7794=CARTESIAN_POINT('Ctrl Pts',(96.7718212348946,0.287951219612599,-1.75277610531714));
#7795=CARTESIAN_POINT('Ctrl Pts',(96.770070542777,0.261961442575343,-1.75691495883756));
#7796=CARTESIAN_POINT('Ctrl Pts',(96.7689129980151,0.244535310882353,-1.75942505076469));
#7797=CARTESIAN_POINT('Ctrl Pts',(96.7631274137211,0.156399475672966,-1.77078545666918));
#7798=CARTESIAN_POINT('Ctrl Pts',(96.7586775786044,0.0852327611901937,-1.77563496365505));
#7799=CARTESIAN_POINT('Ctrl Pts',(96.7462469852487,-0.116088409304546,-1.77721727461864));
#7800=CARTESIAN_POINT('Ctrl Pts',(96.7383913755706,-0.245847526516281,-1.76395441980391));
#7801=CARTESIAN_POINT('Ctrl Pts',(96.7277293221064,-0.4096228602677,-1.72877895969761));
#7802=CARTESIAN_POINT('Ctrl Pts',(96.7253153357333,-0.445990778436983,-1.71975564835071));
#7803=CARTESIAN_POINT('Ctrl Pts',(96.7218596093438,-0.496839121342897,-1.70541820048172));
#7804=CARTESIAN_POINT('Ctrl Pts',(96.7208482201852,-0.511578749778558,-1.70105482254783));
#7805=CARTESIAN_POINT('Ctrl Pts',(96.7189855107789,-0.538451957928767,-1.6927186746764));
#7806=CARTESIAN_POINT('Ctrl Pts',(96.7181361734394,-0.550602990733809,-1.68880530395462));
#7807=CARTESIAN_POINT('Ctrl Pts',(96.7163985709306,-0.575247283188849,-1.68057410707942));
#7808=CARTESIAN_POINT('Ctrl Pts',(96.7155100486443,-0.587736611889357,-1.67624712522501));
#7809=CARTESIAN_POINT('Ctrl Pts',(96.7132714615485,-0.618914248722107,-1.66505422815375));
#7810=CARTESIAN_POINT('Ctrl Pts',(96.7119156399892,-0.637537175345806,-1.65801288404216));
#7811=CARTESIAN_POINT('Ctrl Pts',(96.706188050881,-0.715095985380527,-1.62718796874745));
#7812=CARTESIAN_POINT('Ctrl Pts',(96.7017227651265,-0.772845611352546,-1.60056581526375));
#7813=CARTESIAN_POINT('Ctrl Pts',(96.6871908439572,-0.952443114142012,-1.50578419193227));
#7814=CARTESIAN_POINT('Ctrl Pts',(96.6768203460474,-1.06772991755214,-1.42635256114721));
#7815=CARTESIAN_POINT('Ctrl Pts',(96.6640216999793,-1.20169913623521,-1.30862187833408));
#7816=CARTESIAN_POINT('Ctrl Pts',(96.6612697156964,-1.23002287475852,-1.28203598420486));
#7817=CARTESIAN_POINT('Ctrl Pts',(96.657740092985,-1.26596594136532,-1.24600944134234));
#7818=CARTESIAN_POINT('Ctrl Pts',(96.6569099579442,-1.27439075388407,-1.23739141712105));
#7819=CARTESIAN_POINT('Ctrl Pts',(96.6555701103028,-1.28795157610974,-1.22323417041578));
#7820=CARTESIAN_POINT('Ctrl Pts',(96.6550564979998,-1.2931409524755,-1.21774692794425));
#7821=CARTESIAN_POINT('Ctrl Pts',(96.6540431740179,-1.30336441136377,-1.20679759859031));
#7822=CARTESIAN_POINT('Ctrl Pts',(96.653543395813,-1.30839951827122,-1.20133672943951));
#7823=CARTESIAN_POINT('Ctrl Pts',(96.6522781974598,-1.32112264184425,-1.18736287508338));
#7824=CARTESIAN_POINT('Ctrl Pts',(96.6515162572625,-1.32876288357837,-1.17880653561924));
#7825=CARTESIAN_POINT('Ctrl Pts',(96.6483389712748,-1.360499064883,-1.14256440286425));
#7826=CARTESIAN_POINT('Ctrl Pts',(96.6459739047634,-1.38381854093846,-1.11420725192121));
#7827=CARTESIAN_POINT('Ctrl Pts',(96.6391760797448,-1.44926410057058,-1.02939610599516));
#7828=CARTESIAN_POINT('Ctrl Pts',(96.634843734833,-1.48893365165142,-0.971133725175154));
#7829=CARTESIAN_POINT('Ctrl Pts',(96.6229771282697,-1.58801245031204,-0.805212074532495));
#7830=CARTESIAN_POINT('Ctrl Pts',(96.615469193436,-1.63986946771954,-0.693523012538193));
#7831=CARTESIAN_POINT('Ctrl Pts',(96.605995753295,-1.68765191166171,-0.554508930939387));
#7832=CARTESIAN_POINT('Ctrl Pts',(96.604423331374,-1.6950460714177,-0.53147705045719));
#7833=CARTESIAN_POINT('Ctrl Pts',(96.6018203058615,-1.70639458514099,-0.493478397115742));
#7834=CARTESIAN_POINT('Ctrl Pts',(96.6007987671682,-1.71062782577722,-0.478597769536734));
#7835=CARTESIAN_POINT('Ctrl Pts',(96.5989394484765,-1.71793261651852,-0.451584084712511));
#7836=CARTESIAN_POINT('Ctrl Pts',(96.5981039106108,-1.7210713667691,-0.439470132275238));
#7837=CARTESIAN_POINT('Ctrl Pts',(96.5962915322782,-1.72756889017515,-0.413255236254104));
#7838=CARTESIAN_POINT('Ctrl Pts',(96.5953133346457,-1.73088355559718,-0.399144404723195));
#7839=CARTESIAN_POINT('Ctrl Pts',(96.5925612298575,-1.73967188643625,-0.359561583582922));
#7840=CARTESIAN_POINT('Ctrl Pts',(96.5907751580764,-1.7447581849659,-0.334008316247691));
#7841=CARTESIAN_POINT('Ctrl Pts',(96.5829572510782,-1.76436231667799,-0.222794672062727));
#7842=CARTESIAN_POINT('Ctrl Pts',(96.5767519974262,-1.77314468288618,-0.136256793711199));
#7843=CARTESIAN_POINT('Ctrl Pts',(96.5607332307596,-1.77928215523848,0.0841847312820075));
#7844=CARTESIAN_POINT('Ctrl Pts',(96.5508064275624,-1.76790784823396,0.217799325124803));
#7845=CARTESIAN_POINT('Ctrl Pts',(96.5402093336297,-1.73820508027656,0.3660806167852));
#7846=CARTESIAN_POINT('Ctrl Pts',(96.5389906357336,-1.7345039792407,0.383233509929725));
#7847=CARTESIAN_POINT('Ctrl Pts',(96.5371871673338,-1.72858805696209,0.408806927476766));
#7848=CARTESIAN_POINT('Ctrl Pts',(96.5365925670625,-1.72656465479547,0.417270027035853));
#7849=CARTESIAN_POINT('Ctrl Pts',(96.5355220313824,-1.72278740173632,0.432570746793511));
#7850=CARTESIAN_POINT('Ctrl Pts',(96.5350449616162,-1.72105491804803,0.439413080720304));
#7851=CARTESIAN_POINT('Ctrl Pts',(96.5339631634434,-1.71701400318364,0.454981806028477));
#7852=CARTESIAN_POINT('Ctrl Pts',(96.5333599055038,-1.71467979450505,0.46370113443145));
#7853=CARTESIAN_POINT('Ctrl Pts',(96.5314804346736,-1.70715686030677,0.490968904495373));
#7854=CARTESIAN_POINT('Ctrl Pts',(96.5302167953181,-1.70173266897346,0.509451674044301));
#7855=CARTESIAN_POINT('Ctrl Pts',(96.527220429214,-1.68801680869621,0.553521969975682));
#7856=CARTESIAN_POINT('Ctrl Pts',(96.5255006036531,-1.67944238715746,0.579017045551026));
#7857=CARTESIAN_POINT('Ctrl Pts',(96.5186598692157,-1.64265427280525,0.680698307274408));
#7858=CARTESIAN_POINT('Ctrl Pts',(96.5136926065033,-1.60980699752699,0.755106888657162));
#7859=CARTESIAN_POINT('Ctrl Pts',(96.5021245887605,-1.52206767422841,0.921881756632036));
#7860=CARTESIAN_POINT('Ctrl Pts',(96.4955233611927,-1.46367586985561,1.01203037165438));
#7861=CARTESIAN_POINT('Ctrl Pts',(96.4870251661317,-1.38221816353613,1.11586354820601));
#7862=CARTESIAN_POINT('Ctrl Pts',(96.4854147864763,-1.3665122211505,1.13504306647039));
#7863=CARTESIAN_POINT('Ctrl Pts',(96.4827620665564,-1.34024760626116,1.1657809278241));
#7864=CARTESIAN_POINT('Ctrl Pts',(96.4817294090236,-1.32992811767511,1.17753980546898));
#7865=CARTESIAN_POINT('Ctrl Pts',(96.4798582806115,-1.31106925349879,1.19846500476759));
#7866=CARTESIAN_POINT('Ctrl Pts',(96.4790221868509,-1.30258559149896,1.20768030460096));
#7867=CARTESIAN_POINT('Ctrl Pts',(96.477272054403,-1.28471453510014,1.22668519402338));
#7868=CARTESIAN_POINT('Ctrl Pts',(96.476357353371,-1.27531108684119,1.23645849744996));
#7869=CARTESIAN_POINT('Ctrl Pts',(96.4738375456233,-1.24924077303768,1.26294041246723));
#7870=CARTESIAN_POINT('Ctrl Pts',(96.4722227460352,-1.23235190194515,1.27942553152099));
#7871=CARTESIAN_POINT('Ctrl Pts',(96.468565205041,-1.19371107125203,1.31566755683684));
#7872=CARTESIAN_POINT('Ctrl Pts',(96.4665150914687,-1.17178759817331,1.33523065235273));
#7873=CARTESIAN_POINT('Ctrl Pts',(96.4597987557615,-1.09911985597801,1.39690626094531));
#7874=CARTESIAN_POINT('Ctrl Pts',(96.455054658504,-1.04651757266186,1.43673624852704));
#7875=CARTESIAN_POINT('Ctrl Pts',(96.4430618778972,-0.90974733349233,1.52879473713312));
#7876=CARTESIAN_POINT('Ctrl Pts',(96.4357625293724,-0.823194267332992,1.57708757596209));
#7877=CARTESIAN_POINT('Ctrl Pts',(96.4258284794161,-0.697158952443633,1.63419330722842));
#7878=CARTESIAN_POINT('Ctrl Pts',(96.4230333717317,-0.660713497353632,1.64926546311315));
#7879=CARTESIAN_POINT('Ctrl Pts',(96.4194582617891,-0.61245683148005,1.66736537620701));
#7880=CARTESIAN_POINT('Ctrl Pts',(96.4186241161812,-0.601076381048696,1.67150168194804));
#7881=CARTESIAN_POINT('Ctrl Pts',(96.4172794336662,-0.582518580807284,1.67803259431247));
#7882=CARTESIAN_POINT('Ctrl Pts',(96.4167649467335,-0.575366888624275,1.68049820989801));
#7883=CARTESIAN_POINT('Ctrl Pts',(96.415751437447,-0.561172097585905,1.68529076219419));
#7884=CARTESIAN_POINT('Ctrl Pts',(96.4152523343324,-0.554129784599802,1.68761940674598));
#7885=CARTESIAN_POINT('Ctrl Pts',(96.4139911208785,-0.536208107210804,1.69342119527823));
#7886=CARTESIAN_POINT('Ctrl Pts',(96.4132324462594,-0.525309228327221,1.69683373096838));
#7887=CARTESIAN_POINT('Ctrl Pts',(96.4100895298802,-0.479704720221569,1.71063137956607));
#7888=CARTESIAN_POINT('Ctrl Pts',(96.407754219235,-0.444715976703036,1.7200594334633));
#7889=CARTESIAN_POINT('Ctrl Pts',(96.3967293572918,-0.275739721330435,1.76008990915589));
#7890=CARTESIAN_POINT('Ctrl Pts',(96.3885157802462,-0.138792400966149,1.77614419082633));
#7891=CARTESIAN_POINT('Ctrl Pts',(96.3799606556061,-0.00136080493914694,
1.776249478736));
#7892=CARTESIAN_POINT('Ctrl Pts',(96.3799605315711,-0.00135881241127846,
1.77624948026138));
#7893=CARTESIAN_POINT('Ctrl Pts',(96.3771359461598,0.0440159983497685,1.77628419152053));
#7894=CARTESIAN_POINT('Ctrl Pts',(96.3742821016252,0.0893735997216053,1.77458023586255));
#7895=CARTESIAN_POINT('Ctrl Pts',(96.3695680710927,0.162886034414931,1.76899295676369));
#7896=CARTESIAN_POINT('Ctrl Pts',(96.3677375691263,0.19110043961938,1.7661677226491));
#7897=CARTESIAN_POINT('Ctrl Pts',(96.3649791296725,0.233026948812799,1.76095306372232));
#7898=CARTESIAN_POINT('Ctrl Pts',(96.3640668564934,0.246798975789945,1.75907575138726));
#7899=CARTESIAN_POINT('Ctrl Pts',(96.3623740786795,0.272169704351601,1.75531358069128));
#7900=CARTESIAN_POINT('Ctrl Pts',(96.3615950548584,0.283774538716189,1.75347486850474));
#7901=CARTESIAN_POINT('Ctrl Pts',(96.3599756773798,0.307745227130418,1.74943267727441));
#7902=CARTESIAN_POINT('Ctrl Pts',(96.3591348485344,0.320107624437626,1.74721289827679));
#7903=CARTESIAN_POINT('Ctrl Pts',(96.3572114666753,0.348189162795337,1.74186257801504));
#7904=CARTESIAN_POINT('Ctrl Pts',(96.3561263583703,0.363891364543811,1.73865004505273));
#7905=CARTESIAN_POINT('Ctrl Pts',(96.3532543711735,0.4050708538016,1.72964281694881));
#7906=CARTESIAN_POINT('Ctrl Pts',(96.3514565297596,0.430466670761104,1.72349789391396));
#7907=CARTESIAN_POINT('Ctrl Pts',(96.3426606879059,0.552829861422637,1.6910170651083));
#7908=CARTESIAN_POINT('Ctrl Pts',(96.3354262629305,0.647566284091938,1.65704915401004));
#7909=CARTESIAN_POINT('Ctrl Pts',(96.319717491925,0.843306568021876,1.56750668510802));
#7910=CARTESIAN_POINT('Ctrl Pts',(96.3112477206887,0.942832950861685,1.50973931636731));
#7911=CARTESIAN_POINT('Ctrl Pts',(96.3019566656879,1.05049702935109,1.43242261165794));
#7912=CARTESIAN_POINT('Ctrl Pts',(96.3007246276125,1.06474629232017,1.42186284143817));
#7913=CARTESIAN_POINT('Ctrl Pts',(96.2989054973366,1.08577712208158,1.40578392785827));
#7914=CARTESIAN_POINT('Ctrl Pts',(96.2983083335792,1.09267950405553,1.40042562108768));
#7915=CARTESIAN_POINT('Ctrl Pts',(96.2972830095491,1.10453310351432,1.39108269663284));
#7916=CARTESIAN_POINT('Ctrl Pts',(96.2968532252188,1.10950276963026,1.38712222003486));
#7917=CARTESIAN_POINT('Ctrl Pts',(96.2958449657166,1.12116354053304,1.37772663523553));
#7918=CARTESIAN_POINT('Ctrl Pts',(96.2952680767584,1.12783646352564,1.37226939241132));
#7919=CARTESIAN_POINT('Ctrl Pts',(96.2935544052096,1.14765122798923,1.35582232979771));
#7920=CARTESIAN_POINT('Ctrl Pts',(96.2924272377111,1.16067451617624,1.34469039258165));
#7921=CARTESIAN_POINT('Ctrl Pts',(96.2841349700639,1.25620290138329,1.26061333673786));
#7922=CARTESIAN_POINT('Ctrl Pts',(96.2774143820565,1.33193652298923,1.18031492904804));
#7923=CARTESIAN_POINT('Ctrl Pts',(96.2658271491983,1.44814871144439,1.03155692990616));
#7924=CARTESIAN_POINT('Ctrl Pts',(96.2609953233858,1.49237785151521,0.966463456511067));
#7925=CARTESIAN_POINT('Ctrl Pts',(96.2530029689848,1.55644807866837,0.85722831253604));
#7926=CARTESIAN_POINT('Ctrl Pts',(96.2499279712534,1.57905592553948,0.814832963680922));
#7927=CARTESIAN_POINT('Ctrl Pts',(96.2456070837453,1.60781031903938,0.75520874340931));
#7928=CARTESIAN_POINT('Ctrl Pts',(96.2444127525875,1.61545188814941,0.738721479942792));
#7929=CARTESIAN_POINT('Ctrl Pts',(96.2423568678873,1.62807590441677,0.710351216477564));
#7930=CARTESIAN_POINT('Ctrl Pts',(96.2414997029326,1.63318456213679,0.698525713458277));
#7931=CARTESIAN_POINT('Ctrl Pts',(96.239855242837,1.64268869402638,0.675851252212387));
#7932=CARTESIAN_POINT('Ctrl Pts',(96.2390687588947,1.64710645001301,0.665012324340922));
#7933=CARTESIAN_POINT('Ctrl Pts',(96.2372119112794,1.65723568916024,0.639440075317252));
#7934=CARTESIAN_POINT('Ctrl Pts',(96.2361386277546,1.66285824846726,0.624672839685363));
#7935=CARTESIAN_POINT('Ctrl Pts',(96.2323114358717,1.6820840759176,0.572077914748872));
#7936=CARTESIAN_POINT('Ctrl Pts',(96.2295223155883,1.69459858847406,0.533868105591887));
#7937=CARTESIAN_POINT('Ctrl Pts',(96.217744075585,1.74128313488529,0.373077265965746));
#7938=CARTESIAN_POINT('Ctrl Pts',(96.2084067670488,1.76352441031514,0.247440391240251));
#7939=CARTESIAN_POINT('Ctrl Pts',(96.1950311507562,1.7759607034936,0.0645875547311537));
#7940=CARTESIAN_POINT('Ctrl Pts',(96.1909633780533,1.77711420189509,0.00850086325508087));
#7941=CARTESIAN_POINT('Ctrl Pts',(96.1869838792616,1.77561363799551,-0.0475423081512957));
#7942=CARTESIAN_POINT('Ctrl Pts',(96.0403469459233,1.77561363956144,-0.0475422496666412));
#7943=CARTESIAN_POINT('Ctrl Pts',(96.0429305947739,1.7765607537211,-0.0121693164989692));
#7944=CARTESIAN_POINT('Ctrl Pts',(96.0455230953014,1.77645125620421,0.0232470040897777));
#7945=CARTESIAN_POINT('Ctrl Pts',(96.0536670536774,1.77277018539353,0.134651230012726));
#7946=CARTESIAN_POINT('Ctrl Pts',(96.0591920699511,1.76538228751994,0.210410668352316));
#7947=CARTESIAN_POINT('Ctrl Pts',(96.0657959955279,1.75024958838739,0.303345449978323));
#7948=CARTESIAN_POINT('Ctrl Pts',(96.0670548596476,1.74706544865344,0.321176688500235));
#7949=CARTESIAN_POINT('Ctrl Pts',(96.0689054150075,1.74192774667112,0.347605246776164));
#7950=CARTESIAN_POINT('Ctrl Pts',(96.0695076718102,1.74018215381035,0.356241157197292));
#7951=CARTESIAN_POINT('Ctrl Pts',(96.0705857245962,1.73692306169425,0.371768905423816));
#7952=CARTESIAN_POINT('Ctrl Pts',(96.0710627467569,1.73543268868601,0.378665061297894));
#7953=CARTESIAN_POINT('Ctrl Pts',(96.072136694263,1.73196774586346,0.394247550244933));
#7954=CARTESIAN_POINT('Ctrl Pts',(96.0727322465169,1.72996888680125,0.402928111176793));
#7955=CARTESIAN_POINT('Ctrl Pts',(96.0745623518416,1.72358927002873,0.429710288731958));
#7956=CARTESIAN_POINT('Ctrl Pts',(96.0757852531339,1.718988910735,0.447758971005908));
#7957=CARTESIAN_POINT('Ctrl Pts',(96.0856944615445,1.67901004470484,0.594899098207155));
#7958=CARTESIAN_POINT('Ctrl Pts',(96.0937415366243,1.62942271619631,0.719702123240553));
#7959=CARTESIAN_POINT('Ctrl Pts',(96.1072532047551,1.52601761048561,0.913028002144553));
#7960=CARTESIAN_POINT('Ctrl Pts',(96.112573263114,1.48039082549657,0.985287010657162));
#7961=CARTESIAN_POINT('Ctrl Pts',(96.1197481772966,1.41441283712687,1.07478765958966));
#7962=CARTESIAN_POINT('Ctrl Pts',(96.1214317220378,1.39862358250974,1.09525529010562));
#7963=CARTESIAN_POINT('Ctrl Pts',(96.124083844661,1.37331873206725,1.12661821322305));
#7964=CARTESIAN_POINT('Ctrl Pts',(96.1250403264075,1.3641067679079,1.13775464982094));
#7965=CARTESIAN_POINT('Ctrl Pts',(96.1268355504355,1.34666495163778,1.15832389379713));
#7966=CARTESIAN_POINT('Ctrl Pts',(96.1276728575929,1.33846924430396,1.16778457050768));
#7967=CARTESIAN_POINT('Ctrl Pts',(96.1295581232069,1.3198854016086,1.18878409624206));
#7968=CARTESIAN_POINT('Ctrl Pts',(96.1306082500195,1.30944469720809,1.20027482647593));
#7969=CARTESIAN_POINT('Ctrl Pts',(96.133323738823,1.28222672909368,1.22945228491238));
#7970=CARTESIAN_POINT('Ctrl Pts',(96.134998204742,1.26523403643993,1.24693265100488));
#7971=CARTESIAN_POINT('Ctrl Pts',(96.1447955454228,1.16464765006783,1.34623237311867));
#7972=CARTESIAN_POINT('Ctrl Pts',(96.1532554314745,1.07350776921719,1.41997119366398));
#7973=CARTESIAN_POINT('Ctrl Pts',(96.1672492962213,0.913567196571819,1.52512499028642));
#7974=CARTESIAN_POINT('Ctrl Pts',(96.1727096330583,0.848818828398172,1.5620879575303));
#7975=CARTESIAN_POINT('Ctrl Pts',(96.1798884341912,0.758887891755748,1.60617940948923));
#7976=CARTESIAN_POINT('Ctrl Pts',(96.181712866031,0.735593470474882,1.61698036824198));
#7977=CARTESIAN_POINT('Ctrl Pts',(96.1848209852281,0.695025401393963,1.63473238772244));
#7978=CARTESIAN_POINT('Ctrl Pts',(96.1861150890555,0.677861859100586,1.64192376694141));
#7979=CARTESIAN_POINT('Ctrl Pts',(96.1880068286817,0.652322081780324,1.65215593991399));
#7980=CARTESIAN_POINT('Ctrl Pts',(96.1886156942732,0.644031500587317,1.65540532287018));
#7981=CARTESIAN_POINT('Ctrl Pts',(96.1897003983767,0.629128596796746,1.66111740984336));
#7982=CARTESIAN_POINT('Ctrl Pts',(96.1901775415121,0.622525668807706,1.66360320898977));
#7983=CARTESIAN_POINT('Ctrl Pts',(96.1912454169857,0.607641290655673,1.6691056877951));
#7984=CARTESIAN_POINT('Ctrl Pts',(96.1918348542588,0.599352013488451,1.67210014870824));
#7985=CARTESIAN_POINT('Ctrl Pts',(96.1936263250468,0.573946447942976,1.68106458177001));
#7986=CARTESIAN_POINT('Ctrl Pts',(96.1948174039312,0.556760175894033,1.68683455684777));
#7987=CARTESIAN_POINT('Ctrl Pts',(96.2020621255761,0.450641824788726,1.72066317898613));
#7988=CARTESIAN_POINT('Ctrl Pts',(96.2078058695158,0.359692029100929,1.74194883450128));
#7989=CARTESIAN_POINT('Ctrl Pts',(96.2190111548587,0.179330225747883,1.76942242407391));
#7990=CARTESIAN_POINT('Ctrl Pts',(96.2244597500703,0.0902975448931025,1.77619263733928));
#7991=CARTESIAN_POINT('Ctrl Pts',(96.2332640174644,-0.0496013302610995,
1.77628207226836));
#7992=CARTESIAN_POINT('Ctrl Pts',(96.2365037790513,-0.100312206868422,1.77414064584529));
#7993=CARTESIAN_POINT('Ctrl Pts',(96.2410517104331,-0.169842546179014,1.76821395150884));
#7994=CARTESIAN_POINT('Ctrl Pts',(96.2423023789833,-0.188798532341161,1.76629050181665));
#7995=CARTESIAN_POINT('Ctrl Pts',(96.2443394016273,-0.219382454270107,1.7626892283897));
#7996=CARTESIAN_POINT('Ctrl Pts',(96.245119784636,-0.231031430532863,1.76120028501954));
#7997=CARTESIAN_POINT('Ctrl Pts',(96.2467614032788,-0.255388744886605,1.75784118617991));
#7998=CARTESIAN_POINT('Ctrl Pts',(96.2476233082744,-0.268093229966685,1.75594847642369));
#7999=CARTESIAN_POINT('Ctrl Pts',(96.249701407859,-0.298516383411224,1.75107818949044));
#8000=CARTESIAN_POINT('Ctrl Pts',(96.2509216936409,-0.316212274917905,1.74796928251198));
#8001=CARTESIAN_POINT('Ctrl Pts',(96.2553311850609,-0.379531801574689,1.73585201604046));
#8002=CARTESIAN_POINT('Ctrl Pts',(96.2585677481278,-0.42484132560191,1.72532193241922));
#8003=CARTESIAN_POINT('Ctrl Pts',(96.2671243581273,-0.541597006854946,1.69330956313051));
#8004=CARTESIAN_POINT('Ctrl Pts',(96.272516992436,-0.612191989460444,1.66908465702206));
#8005=CARTESIAN_POINT('Ctrl Pts',(96.2865036993469,-0.789212022949411,1.59559513393595));
#8006=CARTESIAN_POINT('Ctrl Pts',(96.2951473848639,-0.892675143316029,1.5401020788303));
#8007=CARTESIAN_POINT('Ctrl Pts',(96.3044877645388,-1.00352385081625,1.46569849458347));
#8008=CARTESIAN_POINT('Ctrl Pts',(96.3056238031913,-1.0169936440536,1.45638462358153));
#8009=CARTESIAN_POINT('Ctrl Pts',(96.3073370571403,-1.03731557726136,1.44191328793803));
#8010=CARTESIAN_POINT('Ctrl Pts',(96.3079225502138,-1.0442619650909,1.43689056393344));
#8011=CARTESIAN_POINT('Ctrl Pts',(96.3089797874547,-1.05681272686145,1.42767639593554));
#8012=CARTESIAN_POINT('Ctrl Pts',(96.3094526024021,-1.06242890223962,1.42350197125741));
#8013=CARTESIAN_POINT('Ctrl Pts',(96.3105377059455,-1.07532401676266,1.41379838235499));
#8014=CARTESIAN_POINT('Ctrl Pts',(96.3111483870352,-1.08258512229333,1.40824609677859));
#8015=CARTESIAN_POINT('Ctrl Pts',(96.3130763915856,-1.10550813790064,1.39043567151691));
#8016=CARTESIAN_POINT('Ctrl Pts',(96.3143801998682,-1.12100779813375,1.37796995504197));
#8017=CARTESIAN_POINT('Ctrl Pts',(96.3174917772527,-1.15788567820576,1.34727645706107));
#8018=CARTESIAN_POINT('Ctrl Pts',(96.3192852768906,-1.17904766352649,1.32879640039378));
#8019=CARTESIAN_POINT('Ctrl Pts',(96.3266447849985,-1.26497907830156,1.25008537108752));
#8020=CARTESIAN_POINT('Ctrl Pts',(96.3320328771673,-1.32564632861231,1.18555864382153));
#8021=CARTESIAN_POINT('Ctrl Pts',(96.3440149301448,-1.44826292070771,1.03390349240651));
#8022=CARTESIAN_POINT('Ctrl Pts',(96.3506131582488,-1.50766587335273,0.945178043956437));
#8023=CARTESIAN_POINT('Ctrl Pts',(96.3589860392484,-1.5696110079357,0.831803977510228));
#8024=CARTESIAN_POINT('Ctrl Pts',(96.3604655216718,-1.58008451500923,0.811732359071696));
#8025=CARTESIAN_POINT('Ctrl Pts',(96.3628674593071,-1.59631312264466,0.779126739895723));
#8026=CARTESIAN_POINT('Ctrl Pts',(96.3637813830707,-1.60231105673727,0.766715932849892));
#8027=CARTESIAN_POINT('Ctrl Pts',(96.3655429361139,-1.61353013802961,0.742794905873446));
#8028=CARTESIAN_POINT('Ctrl Pts',(96.3663897100565,-1.61877408507284,0.731296263990779));
#8029=CARTESIAN_POINT('Ctrl Pts',(96.3683634329026,-1.6306500609846,0.704501508135821));
#8030=CARTESIAN_POINT('Ctrl Pts',(96.3694934375602,-1.63719023074581,0.68916624379013));
#8031=CARTESIAN_POINT('Ctrl Pts',(96.3732127549297,-1.65786798179438,0.638725305186988));
#8032=CARTESIAN_POINT('Ctrl Pts',(96.3758318742429,-1.67109881218692,0.603261670587379));
#8033=CARTESIAN_POINT('Ctrl Pts',(96.3823112229407,-1.70061124914197,0.515714072397891));
#8034=CARTESIAN_POINT('Ctrl Pts',(96.3862060737616,-1.71564442895074,0.463252513849962));
#8035=CARTESIAN_POINT('Ctrl Pts',(96.3920633671962,-1.73435957616409,0.384399954820618));
#8036=CARTESIAN_POINT('Ctrl Pts',(96.3939889571552,-1.73990180156531,0.358480295225153));
#8037=CARTESIAN_POINT('Ctrl Pts',(96.4041006893171,-1.76586579546782,0.222207165366694));
#8038=CARTESIAN_POINT('Ctrl Pts',(96.4123882134443,-1.77637602342196,0.110220894126013));
#8039=CARTESIAN_POINT('Ctrl Pts',(96.4219356337484,-1.77622292108002,-0.0249058862137763));
#8040=CARTESIAN_POINT('Ctrl Pts',(96.4235367073418,-1.77575438786865,-0.0477979414076611));
#8041=CARTESIAN_POINT('Ctrl Pts',(96.4257369128305,-1.77448549307923,-0.0796630104551556));
#8042=CARTESIAN_POINT('Ctrl Pts',(96.4263541214217,-1.77405934820833,-0.0886476058793519));
#8043=CARTESIAN_POINT('Ctrl Pts',(96.4274592574622,-1.77316887393021,-0.104824326006481));
#8044=CARTESIAN_POINT('Ctrl Pts',(96.4279484807638,-1.77272898713365,-0.11201758910826));
#8045=CARTESIAN_POINT('Ctrl Pts',(96.4289580706819,-1.77172574007857,-0.126932662859727));
#8046=CARTESIAN_POINT('Ctrl Pts',(96.4294780672173,-1.77115565795979,-0.134653778236111));
#8047=CARTESIAN_POINT('Ctrl Pts',(96.430859039143,-1.76949909525797,-0.15525488560299));
#8048=CARTESIAN_POINT('Ctrl Pts',(96.4317151909711,-1.76832245787829,-0.168127442025727));
#8049=CARTESIAN_POINT('Ctrl Pts',(96.4361606407028,-1.76143035413475,-0.235416363585029));
#8050=CARTESIAN_POINT('Ctrl Pts',(96.4396357816746,-1.75334276350391,-0.289565461497547));
#8051=CARTESIAN_POINT('Ctrl Pts',(96.4518478839361,-1.7155738740101,-0.48132212391297));
#8052=CARTESIAN_POINT('Ctrl Pts',(96.4602674316417,-1.67207244681705,-0.615662730493593));
#8053=CARTESIAN_POINT('Ctrl Pts',(96.4721491277466,-1.59324143018987,-0.786710336662938));
#8054=CARTESIAN_POINT('Ctrl Pts',(96.4751958222187,-1.57158171838095,-0.829133103648108));
#8055=CARTESIAN_POINT('Ctrl Pts',(96.4795158378172,-1.53911593211159,-0.886867033379799));
#8056=CARTESIAN_POINT('Ctrl Pts',(96.4807392228008,-1.52973190582593,-0.902956942727873));
#8057=CARTESIAN_POINT('Ctrl Pts',(96.4827440000593,-1.51405971622055,-0.928882892035104));
#8058=CARTESIAN_POINT('Ctrl Pts',(96.4835197970066,-1.50792440146361,-0.93881001261809));
#8059=CARTESIAN_POINT('Ctrl Pts',(96.485161869898,-1.49479355162338,-0.959595291276738));
#8060=CARTESIAN_POINT('Ctrl Pts',(96.4860289095425,-1.48777653469146,-0.97043899990679));
#8061=CARTESIAN_POINT('Ctrl Pts',(96.4881393193162,-1.47049946272533,-0.996510167248802));
#8062=CARTESIAN_POINT('Ctrl Pts',(96.4893871067741,-1.46012052952907,-1.01165665040451));
#8063=CARTESIAN_POINT('Ctrl Pts',(96.4940313797154,-1.42090299781262,-1.06702778179582));
#8064=CARTESIAN_POINT('Ctrl Pts',(96.49748219682,-1.39062410456743,-1.10619952662017));
#8065=CARTESIAN_POINT('Ctrl Pts',(96.5068460732315,-1.30549852244011,-1.20730020674722));
#8066=CARTESIAN_POINT('Ctrl Pts',(96.5128512574472,-1.24789914464058,-1.26674600555088));
#8067=CARTESIAN_POINT('Ctrl Pts',(96.5264416373767,-1.10953018681088,-1.3909234703311));
#8068=CARTESIAN_POINT('Ctrl Pts',(96.5340262472109,-1.02681155116719,-1.45306120981445));
#8069=CARTESIAN_POINT('Ctrl Pts',(96.5425050795468,-0.924134324972083,-1.51702111036533));
#8070=CARTESIAN_POINT('Ctrl Pts',(96.5437346179634,-0.908972255393016,-1.52615425114478));
#8071=CARTESIAN_POINT('Ctrl Pts',(96.5455508018133,-0.886130283236608,-1.53945230824795));
#8072=CARTESIAN_POINT('Ctrl Pts',(96.5461474734486,-0.878552575863178,-1.54378938582509));
#8073=CARTESIAN_POINT('Ctrl Pts',(96.5472200098624,-0.864792511976391,-1.55153078461017));
#8074=CARTESIAN_POINT('Ctrl Pts',(96.5476970340651,-0.858621571191204,-1.55495429702979));
#8075=CARTESIAN_POINT('Ctrl Pts',(96.5487765738756,-0.844540855101335,-1.5626566062066));
#8076=CARTESIAN_POINT('Ctrl Pts',(96.5493776464294,-0.836618809330666,-1.56691221880814));
#8077=CARTESIAN_POINT('Ctrl Pts',(96.551243080958,-0.811789057644641,-1.58000841642962));
#8078=CARTESIAN_POINT('Ctrl Pts',(96.5524951347937,-0.794770389611333,-1.58863720526073));
#8079=CARTESIAN_POINT('Ctrl Pts',(96.5554585327273,-0.753742116818432,-1.60861491124368));
#8080=CARTESIAN_POINT('Ctrl Pts',(96.5571573528449,-0.729610139254469,-1.61970315313515));
#8081=CARTESIAN_POINT('Ctrl Pts',(96.5638571617283,-0.632460043549448,-1.66172984783569));
#8082=CARTESIAN_POINT('Ctrl Pts',(96.5687108282092,-0.557651250579835,-1.68830641348407));
#8083=CARTESIAN_POINT('Ctrl Pts',(96.5803478917882,-0.375155249633172,-1.73967956813267));
#8084=CARTESIAN_POINT('Ctrl Pts',(96.5871305227646,-0.266457729055983,-1.7596087985455));
#8085=CARTESIAN_POINT('Ctrl Pts',(96.5958125007933,-0.132207570211483,-1.77149255555919));
#8086=CARTESIAN_POINT('Ctrl Pts',(96.5974051789182,-0.107753695154972,-1.77314798134366));
#8087=CARTESIAN_POINT('Ctrl Pts',(96.600034712005,-0.0677279813718079,-1.77502653611153));
#8088=CARTESIAN_POINT('Ctrl Pts',(96.6010621743621,-0.0521731590333654,
-1.77555180693419));
#8089=CARTESIAN_POINT('Ctrl Pts',(96.6029277325171,-0.024097086011011,-1.77613066209162));
#8090=CARTESIAN_POINT('Ctrl Pts',(96.6037635139506,-0.0115782317456789,
-1.77625638045931));
#8091=CARTESIAN_POINT('Ctrl Pts',(96.6055712791055,0.0153650730629895,-1.77624211229682));
#8092=CARTESIAN_POINT('Ctrl Pts',(96.606544562844,0.0297884983151368,-1.77605876899343));
#8093=CARTESIAN_POINT('Ctrl Pts',(96.6092681825941,0.0699110680632635,-1.77505987962055));
#8094=CARTESIAN_POINT('Ctrl Pts',(96.6110302787581,0.0955962382527541,-1.77386199356287));
#8095=CARTESIAN_POINT('Ctrl Pts',(96.6186465448605,0.205403068147676,-1.76634915506463));
#8096=CARTESIAN_POINT('Ctrl Pts',(96.6246636818704,0.289032029862484,-1.75460441867524));
#8097=CARTESIAN_POINT('Ctrl Pts',(96.640089302414,0.496909221935101,-1.71014389116129));
#8098=CARTESIAN_POINT('Ctrl Pts',(96.6496061101153,0.619044508931569,-1.66981919887867));
#8099=CARTESIAN_POINT('Ctrl Pts',(96.6602723154879,0.756472068764938,-1.607274458543));
#8100=CARTESIAN_POINT('Ctrl Pts',(96.6618624219181,0.776987924297431,-1.59745768641492));
#8101=CARTESIAN_POINT('Ctrl Pts',(96.6640501907187,0.805326124750116,-1.58322277429939));
#8102=CARTESIAN_POINT('Ctrl Pts',(96.6646656761367,0.813311121542918,-1.57913569663409));
#8103=CARTESIAN_POINT('Ctrl Pts',(96.6657686595379,0.827649421922248,-1.57165910435213));
#8104=CARTESIAN_POINT('Ctrl Pts',(96.6662574377991,0.83401371977274,-1.56829111725617));
#8105=CARTESIAN_POINT('Ctrl Pts',(96.6672673201938,0.847188129075107,-1.56121633576739));
#8106=CARTESIAN_POINT('Ctrl Pts',(96.6677880423197,0.853994723795976,-1.55750351223451));
#8107=CARTESIAN_POINT('Ctrl Pts',(96.6691731381417,0.8721284908976,-1.54745738675956));
#8108=CARTESIAN_POINT('Ctrl Pts',(96.6700326376638,0.883411183373555,-1.54104418301764));
#8109=CARTESIAN_POINT('Ctrl Pts',(96.6745377654946,0.942637930946875,-1.50651479581373));
#8110=CARTESIAN_POINT('Ctrl Pts',(96.6780655359865,0.989317791106444,-1.47628069982322));
#8111=CARTESIAN_POINT('Ctrl Pts',(96.689945931623,1.14396695557424,-1.36547992972549));
#8112=CARTESIAN_POINT('Ctrl Pts',(96.6980172235576,1.24415374654073,-1.27486438901223));
#8113=CARTESIAN_POINT('Ctrl Pts',(96.7097268330864,1.36718145418235,-1.13513535636418));
#8114=CARTESIAN_POINT('Ctrl Pts',(96.7130144029842,1.39952055358183,-1.09501546842448));
#8115=CARTESIAN_POINT('Ctrl Pts',(96.7176183032336,1.44142704974603,-1.0381323763672));
#8116=CARTESIAN_POINT('Ctrl Pts',(96.7188751648333,1.45253485041673,-1.02253275354074));
#8117=CARTESIAN_POINT('Ctrl Pts',(96.7209195284333,1.47005376763467,-0.997067849906867));
#8118=CARTESIAN_POINT('Ctrl Pts',(96.7217009729549,1.47662306765102,-0.987312859135083));
#8119=CARTESIAN_POINT('Ctrl Pts',(96.7233426119769,1.49015535386034,-0.966781097631948));
#8120=CARTESIAN_POINT('Ctrl Pts',(96.7242034552566,1.49709938928443,-0.955992715975454));
#8121=CARTESIAN_POINT('Ctrl Pts',(96.7262747434513,1.51344123132743,-0.929988981057599));
#8122=CARTESIAN_POINT('Ctrl Pts',(96.7274892112717,1.52272715137805,-0.914705333504172));
#8123=CARTESIAN_POINT('Ctrl Pts',(96.7318506890216,1.55501601619991,-0.859706667257943));
#8124=CARTESIAN_POINT('Ctrl Pts',(96.735043694123,1.5767069529734,-0.819246536161576));
#8125=CARTESIAN_POINT('Ctrl Pts',(96.7434425754164,1.62878217932912,-0.712364092350434));
#8126=CARTESIAN_POINT('Ctrl Pts',(96.7487175546672,1.65667916698548,-0.644830401763326));
#8127=CARTESIAN_POINT('Ctrl Pts',(96.7627968283574,1.71924971914142,-0.46222569635848));
#8128=CARTESIAN_POINT('Ctrl Pts',(96.7716645787291,1.7465511271665,-0.345014884656039));
#8129=CARTESIAN_POINT('Ctrl Pts',(96.7811810998427,1.76386280466687,-0.210022825954433));
#8130=CARTESIAN_POINT('Ctrl Pts',(96.7822939260873,1.76568833496166,-0.194078154182664));
#8131=CARTESIAN_POINT('Ctrl Pts',(96.7839794602016,1.76815013766352,-0.169650935814082));
#8132=CARTESIAN_POINT('Ctrl Pts',(96.7845600632623,1.76894195155957,-0.161185386670087));
#8133=CARTESIAN_POINT('Ctrl Pts',(96.7856173569261,1.77028092814129,-0.145669149656872));
#8134=CARTESIAN_POINT('Ctrl Pts',(96.786095012061,1.77084679814569,-0.138620656056731));
#8135=CARTESIAN_POINT('Ctrl Pts',(96.7871934042979,1.77205718347817,-0.122324659259793));
#8136=CARTESIAN_POINT('Ctrl Pts',(96.7878124725179,1.77267142432164,-0.113075261067244));
#8137=CARTESIAN_POINT('Ctrl Pts',(96.7896744186737,1.7743107609307,-0.0850762327700656));
#8138=CARTESIAN_POINT('Ctrl Pts',(96.7909057720709,1.77511101730436,-0.0663142284229205));
#8139=CARTESIAN_POINT('Ctrl Pts',(96.7921246218182,1.77561363837209,-0.0475422940869062));
#8140=CARTESIAN_POINT('Origin',(88.3562164250559,0.,0.));
#8141=CARTESIAN_POINT('',(97.6892780485025,1.77561363630377,-0.0475423713344133));
#8142=CARTESIAN_POINT('',(97.5395353031289,1.77561364475627,-0.0475420556493824));
#8143=CARTESIAN_POINT('',(88.3562164250559,1.77561363837197,-0.0475422940912398));
#8144=CARTESIAN_POINT('Ctrl Pts',(97.6892780485025,1.77561363630377,-0.0475423713344133));
#8145=CARTESIAN_POINT('Ctrl Pts',(97.6860851367942,1.7742455753338,-0.098636745581963));
#8146=CARTESIAN_POINT('Ctrl Pts',(97.6828502987857,1.77067243241096,-0.149661107924927));
#8147=CARTESIAN_POINT('Ctrl Pts',(97.6778872795951,1.76199269377043,-0.226074449728626));
#8148=CARTESIAN_POINT('Ctrl Pts',(97.6762089950545,1.75852819260191,-0.251607622260889));
#8149=CARTESIAN_POINT('Ctrl Pts',(97.6735632941531,1.75225805166211,-0.291314566887335));
#8150=CARTESIAN_POINT('Ctrl Pts',(97.6726078751094,1.74983269179659,-0.30554539190279));
#8151=CARTESIAN_POINT('Ctrl Pts',(97.6708135629497,1.74498066720861,-0.332059115408676));
#8152=CARTESIAN_POINT('Ctrl Pts',(97.6699760909007,1.74259705634423,-0.344349053175954));
#8153=CARTESIAN_POINT('Ctrl Pts',(97.668089017505,1.73696201122558,-0.371845146531463));
#8154=CARTESIAN_POINT('Ctrl Pts',(97.6670372296867,1.73364044114145,-0.38703570302432));
#8155=CARTESIAN_POINT('Ctrl Pts',(97.6643144480537,1.72458210704467,-0.426003313583445));
#8156=CARTESIAN_POINT('Ctrl Pts',(97.6626342676826,1.71855304858058,-0.449708330764711));
#8157=CARTESIAN_POINT('Ctrl Pts',(97.6530897555053,1.68186805120106,-0.58241205918583));
#8158=CARTESIAN_POINT('Ctrl Pts',(97.6449119597441,1.64133880184685,-0.688391596023122));
#8159=CARTESIAN_POINT('Ctrl Pts',(97.6310005188252,1.55670350694662,-0.858889850223094));
#8160=CARTESIAN_POINT('Ctrl Pts',(97.6253386875275,1.51792806652487,-0.925695892344974));
#8161=CARTESIAN_POINT('Ctrl Pts',(97.6179279154381,1.46034812331345,-1.01149997829049));
#8162=CARTESIAN_POINT('Ctrl Pts',(97.6160671760906,1.44528724671633,-1.03290549710349));
#8163=CARTESIAN_POINT('Ctrl Pts',(97.6129042420688,1.41855892678731,-1.06916362510806));
#8164=CARTESIAN_POINT('Ctrl Pts',(97.6115911680215,1.40711775137802,-1.08417710314031));
#8165=CARTESIAN_POINT('Ctrl Pts',(97.6096772980609,1.3898985829476,-1.10604076472857));
#8166=CARTESIAN_POINT('Ctrl Pts',(97.609064907682,1.38430501417714,-1.11303363855099));
#8167=CARTESIAN_POINT('Ctrl Pts',(97.6079765881981,1.37420938251813,-1.12546098455746));
#8168=CARTESIAN_POINT('Ctrl Pts',(97.6074993130242,1.36972755906712,-1.13091125804803));
#8169=CARTESIAN_POINT('Ctrl Pts',(97.6064343912579,1.35960498133772,-1.14307270331917));
#8170=CARTESIAN_POINT('Ctrl Pts',(97.6058480004248,1.35394690022151,-1.14976898107994));
#8171=CARTESIAN_POINT('Ctrl Pts',(97.6040756557549,1.33659758303948,-1.16999603141518));
#8172=CARTESIAN_POINT('Ctrl Pts',(97.6029003189752,1.32475099769636,-1.18339286237959));
#8173=CARTESIAN_POINT('Ctrl Pts',(97.5954625188914,1.24775107531066,-1.26786328036346));
#8174=CARTESIAN_POINT('Ctrl Pts',(97.5895337426477,1.17709629497725,-1.33371998978517));
#8175=CARTESIAN_POINT('Ctrl Pts',(97.5806755662456,1.06391453497321,-1.42317861191845));
#8176=CARTESIAN_POINT('Ctrl Pts',(97.5777455429909,1.02521054317239,-1.4513079431965));
#8177=CARTESIAN_POINT('Ctrl Pts',(97.5713205616504,0.938716378206845,-1.50898195869091));
#8178=CARTESIAN_POINT('Ctrl Pts',(97.5678191601895,0.890566680024818,-1.5378898829842));
#8179=CARTESIAN_POINT('Ctrl Pts',(97.5617913582137,0.807132920930405,-1.58274778755483));
#8180=CARTESIAN_POINT('Ctrl Pts',(97.5593039128058,0.772549516970274,-1.59991281346182));
#8181=CARTESIAN_POINT('Ctrl Pts',(97.555678680275,0.722157435175025,-1.6229093512226));
#8182=CARTESIAN_POINT('Ctrl Pts',(97.554572438951,0.706780878128642,-1.6296646531436));
#8183=CARTESIAN_POINT('Ctrl Pts',(97.5526195067215,0.679653569629399,-1.64112621400613));
#8184=CARTESIAN_POINT('Ctrl Pts',(97.5517760901293,0.66794382794548,-1.64592686760696));
#8185=CARTESIAN_POINT('Ctrl Pts',(97.5500087152771,0.643425160313609,-1.65567407475106));
#8186=CARTESIAN_POINT('Ctrl Pts',(97.5490840624209,0.630608219265672,-1.66059803507056));
#8187=CARTESIAN_POINT('Ctrl Pts',(97.546638934068,0.596752388612501,-1.67315615919371));
#8188=CARTESIAN_POINT('Ctrl Pts',(97.5451103431152,0.575624640443485,-1.68054191847934));
#8189=CARTESIAN_POINT('Ctrl Pts',(97.5367581266179,0.46043481555503,-1.71838255638424));
#8190=CARTESIAN_POINT('Ctrl Pts',(97.5296940642403,0.364109062153793,-1.74133788960204));
#8191=CARTESIAN_POINT('Ctrl Pts',(97.5166888289907,0.18737235502855,-1.76814674305959));
#8192=CARTESIAN_POINT('Ctrl Pts',(97.5108099048211,0.107638023393683,-1.77478598852511));
#8193=CARTESIAN_POINT('Ctrl Pts',(97.5009453103086,-0.0284251646162766,
-1.77691024142284));
#8194=CARTESIAN_POINT('Ctrl Pts',(97.4969232324965,-0.0845942238383299,
-1.77512340432486));
#8195=CARTESIAN_POINT('Ctrl Pts',(97.4921148464802,-0.153559953124779,-1.76964762039276));
#8196=CARTESIAN_POINT('Ctrl Pts',(97.4912170293429,-0.166519331224918,-1.76847524633837));
#8197=CARTESIAN_POINT('Ctrl Pts',(97.4897956201097,-0.187186139931326,-1.76637641526618));
#8198=CARTESIAN_POINT('Ctrl Pts',(97.4892672493625,-0.194902120250317,-1.76554169045786));
#8199=CARTESIAN_POINT('Ctrl Pts',(97.488254441058,-0.209762345949854,-1.76383548381618));
#8200=CARTESIAN_POINT('Ctrl Pts',(97.4877696507699,-0.216907112276236,-1.76297111788326));
#8201=CARTESIAN_POINT('Ctrl Pts',(97.4866869910549,-0.232929453070199,-1.76093387564777));
#8202=CARTESIAN_POINT('Ctrl Pts',(97.4860904219326,-0.24180394109597,-1.75973722668616));
#8203=CARTESIAN_POINT('Ctrl Pts',(97.4839972776029,-0.273085972637487,-1.75527799379606));
#8204=CARTESIAN_POINT('Ctrl Pts',(97.4825191052179,-0.295440827975233,-1.75165396585247));
#8205=CARTESIAN_POINT('Ctrl Pts',(97.4727772573635,-0.443995740595216,-1.72464606865087));
#8206=CARTESIAN_POINT('Ctrl Pts',(97.46505321923,-0.567424474727915,-1.68806801141452));
#8207=CARTESIAN_POINT('Ctrl Pts',(97.451937575724,-0.763672693581614,-1.60592239649487));
#8208=CARTESIAN_POINT('Ctrl Pts',(97.4466757615812,-0.839073408649331,-1.56784444489353));
#8209=CARTESIAN_POINT('Ctrl Pts',(97.4395717900887,-0.933548914404199,-1.51136088335045));
#8210=CARTESIAN_POINT('Ctrl Pts',(97.437896729353,-0.955329522485675,-1.49768844871949));
#8211=CARTESIAN_POINT('Ctrl Pts',(97.4352549778074,-0.988853125566246,-1.47561568557153));
#8212=CARTESIAN_POINT('Ctrl Pts',(97.434300224079,-1.00080404708521,-1.46753650521054));
#8213=CARTESIAN_POINT('Ctrl Pts',(97.4325065027749,-1.02294087606994,-1.45217518680701));
#8214=CARTESIAN_POINT('Ctrl Pts',(97.4316689476699,-1.03315081579598,-1.44492912873749));
#8215=CARTESIAN_POINT('Ctrl Pts',(97.4297808120678,-1.05587907306941,-1.42843469094478));
#8216=CARTESIAN_POINT('Ctrl Pts',(97.4287280341355,-1.06835401452044,-1.41912859035445));
#8217=CARTESIAN_POINT('Ctrl Pts',(97.4260008607048,-1.10015403665477,-1.3947493545123));
#8218=CARTESIAN_POINT('Ctrl Pts',(97.4243172284351,-1.11929178981383,-1.37943845507715));
#8219=CARTESIAN_POINT('Ctrl Pts',(97.414966201394,-1.22284828997991,-1.29301545342972));
#8220=CARTESIAN_POINT('Ctrl Pts',(97.4070025974125,-1.30080083094552,-1.21456030540418));
#8221=CARTESIAN_POINT('Ctrl Pts',(97.3931521974554,-1.42133975248412,-1.06823942455043));
#8222=CARTESIAN_POINT('Ctrl Pts',(97.387334266965,-1.46757267273331,-1.00377960977377));
#8223=CARTESIAN_POINT('Ctrl Pts',(97.3797445969987,-1.52334126397546,-0.91389272769813));
#8224=CARTESIAN_POINT('Ctrl Pts',(97.3778565238841,-1.53682765047578,-0.891027186070993));
#8225=CARTESIAN_POINT('Ctrl Pts',(97.3746524303853,-1.55911624108677,-0.851225232666872));
#8226=CARTESIAN_POINT('Ctrl Pts',(97.3733251762329,-1.56816714668493,-0.834433774077758));
#8227=CARTESIAN_POINT('Ctrl Pts',(97.371394798285,-1.58108448748137,-0.809516369581118));
#8228=CARTESIAN_POINT('Ctrl Pts',(97.3707798040096,-1.58516215472815,-0.801502252769358));
#8229=CARTESIAN_POINT('Ctrl Pts',(97.3696888056598,-1.59233138940458,-0.787143324507735));
#8230=CARTESIAN_POINT('Ctrl Pts',(97.3692114248528,-1.59544619965415,-0.780810665933484));
#8231=CARTESIAN_POINT('Ctrl Pts',(97.3681486391894,-1.60233067676083,-0.766600754156208));
#8232=CARTESIAN_POINT('Ctrl Pts',(97.3675644615615,-1.60608008853077,-0.758714090563911));
#8233=CARTESIAN_POINT('Ctrl Pts',(97.3658058854859,-1.61725503490599,-0.734754167266526));
#8234=CARTESIAN_POINT('Ctrl Pts',(97.3646418645835,-1.62449880927977,-0.718596695903648));
#8235=CARTESIAN_POINT('Ctrl Pts',(97.3548441005699,-1.68401395711633,-0.580344630162377));
#8236=CARTESIAN_POINT('Ctrl Pts',(97.3468508091913,-1.72268794946102,-0.452834486244263));
#8237=CARTESIAN_POINT('Ctrl Pts',(97.3338630160027,-1.76093808214626,-0.245457280220734));
#8238=CARTESIAN_POINT('Ctrl Pts',(97.3290119156321,-1.7700185981609,-0.167882842248317));
#8239=CARTESIAN_POINT('Ctrl Pts',(97.3219751714822,-1.77558103311633,-0.0582032388153459));
#8240=CARTESIAN_POINT('Ctrl Pts',(97.3199147583734,-1.77633845114438,-0.026403202290071));
#8241=CARTESIAN_POINT('Ctrl Pts',(97.3168032564605,-1.77619432741937,0.0210168398053602));
#8242=CARTESIAN_POINT('Ctrl Pts',(97.3157722796422,-1.77594086713687,0.0366334103178855));
#8243=CARTESIAN_POINT('Ctrl Pts',(97.3139029481796,-1.77511315781711,0.0647625144756611));
#8244=CARTESIAN_POINT('Ctrl Pts',(97.3130669502636,-1.77461242710866,0.0772762969659785));
#8245=CARTESIAN_POINT('Ctrl Pts',(97.3112616440601,-1.77325227257266,0.104150800846863));
#8246=CARTESIAN_POINT('Ctrl Pts',(97.3102910679666,-1.77235062903052,0.118508388028271));
#8247=CARTESIAN_POINT('Ctrl Pts',(97.3076293381081,-1.76941664928055,0.157625916758776));
#8248=CARTESIAN_POINT('Ctrl Pts',(97.3059275397609,-1.76703917022971,0.18235588917505));
#8249=CARTESIAN_POINT('Ctrl Pts',(97.2944875463846,-1.74775628799199,0.346671704171294));
#8250=CARTESIAN_POINT('Ctrl Pts',(97.2842387785549,-1.71484836886303,0.483853147740892));
#8251=CARTESIAN_POINT('Ctrl Pts',(97.2695889457956,-1.64538395672542,0.671831720883208));
#8252=CARTESIAN_POINT('Ctrl Pts',(97.2652269375064,-1.62181263006219,0.726891206554976));
#8253=CARTESIAN_POINT('Ctrl Pts',(97.258574357595,-1.58086144958288,0.810587017625067));
#8254=CARTESIAN_POINT('Ctrl Pts',(97.2562243807072,-1.56537732742084,0.840100230408765));
#8255=CARTESIAN_POINT('Ctrl Pts',(97.2531504459254,-1.54364110389789,0.87883976818607));
#8256=CARTESIAN_POINT('Ctrl Pts',(97.2523875043142,-1.53812055206124,0.888466307219416));
#8257=CARTESIAN_POINT('Ctrl Pts',(97.2511283718436,-1.52879356342425,0.904382848350329));
#8258=CARTESIAN_POINT('Ctrl Pts',(97.2506290923629,-1.52503770716857,0.910701979105579));
#8259=CARTESIAN_POINT('Ctrl Pts',(97.2496155028211,-1.51729300760363,0.923549956016718));
#8260=CARTESIAN_POINT('Ctrl Pts',(97.2491014010215,-1.51330103134567,0.930076656133694));
#8261=CARTESIAN_POINT('Ctrl Pts',(97.2477539924649,-1.50267385867069,0.947202030026113));
#8262=CARTESIAN_POINT('Ctrl Pts',(97.2469251046745,-1.4959685661537,0.957757005886478));
#8263=CARTESIAN_POINT('Ctrl Pts',(97.2432177592273,-1.46524950761932,1.00500285444358));
#8264=CARTESIAN_POINT('Ctrl Pts',(97.2404110674975,-1.43999156109458,1.04087071867133));
#8265=CARTESIAN_POINT('Ctrl Pts',(97.2316173425303,-1.35543808043715,1.15196361958598));
#8266=CARTESIAN_POINT('Ctrl Pts',(97.2258050666096,-1.29137734948703,1.22334755089961));
#8267=CARTESIAN_POINT('Ctrl Pts',(97.2144259797327,-1.15721222554527,1.35050363808496));
#8268=CARTESIAN_POINT('Ctrl Pts',(97.2088860335297,-1.08804190118155,1.40682708479119));
#8269=CARTESIAN_POINT('Ctrl Pts',(97.2014432529643,-0.993323652236097,1.47277500882813));
#8270=CARTESIAN_POINT('Ctrl Pts',(97.1997281982726,-0.971372019795175,1.48734474373017));
#8271=CARTESIAN_POINT('Ctrl Pts',(97.197037468463,-0.936802927122869,1.50919719333448));
#8272=CARTESIAN_POINT('Ctrl Pts',(97.1960744872528,-0.924405663805522,1.51682234957224));
#8273=CARTESIAN_POINT('Ctrl Pts',(97.1942733451361,-0.901181239050674,1.53071647515727));
#8274=CARTESIAN_POINT('Ctrl Pts',(97.1934367022838,-0.890378775346953,1.53702510569225));
#8275=CARTESIAN_POINT('Ctrl Pts',(97.1915611397493,-0.866136092175699,1.55084148712438));
#8276=CARTESIAN_POINT('Ctrl Pts',(97.1905201533219,-0.852663226102643,1.5582895896279));
#8277=CARTESIAN_POINT('Ctrl Pts',(97.1878451286312,-0.818007712317258,1.57686394194831));
#8278=CARTESIAN_POINT('Ctrl Pts',(97.1862024419064,-0.796694542136727,1.58773871223062));
#8279=CARTESIAN_POINT('Ctrl Pts',(97.175715937046,-0.660490524407602,1.6538021068581));
#8280=CARTESIAN_POINT('Ctrl Pts',(97.166463225868,-0.540177302808986,1.69691092413055));
#8281=CARTESIAN_POINT('Ctrl Pts',(97.1522132162331,-0.350766428870102,1.74257655893968));
#8282=CARTESIAN_POINT('Ctrl Pts',(97.1472830034468,-0.284369881230242,1.75463524134333));
#8283=CARTESIAN_POINT('Ctrl Pts',(97.1398974533419,-0.181926266547648,1.76727126281748));
#8284=CARTESIAN_POINT('Ctrl Pts',(97.1373685041337,-0.14627965715846,1.77057831064361));
#8285=CARTESIAN_POINT('Ctrl Pts',(97.134102278792,-0.0992036183010982,1.77351404131004));
#8286=CARTESIAN_POINT('Ctrl Pts',(97.1333198709273,-0.0878455342175128,
1.77411290278429));
#8287=CARTESIAN_POINT('Ctrl Pts',(97.1320374642849,-0.0690816861468553,
1.77492159014721));
#8288=CARTESIAN_POINT('Ctrl Pts',(97.131534146549,-0.0616791231231223,1.77519424929974));
#8289=CARTESIAN_POINT('Ctrl Pts',(97.1305834792549,-0.0476203873594082,
1.77562402678054));
#8290=CARTESIAN_POINT('Ctrl Pts',(97.1301356227535,-0.0409646935344745,
1.77579004484116));
#8291=CARTESIAN_POINT('Ctrl Pts',(97.1289339825993,-0.0230240468821298,
1.77613663123154));
#8292=CARTESIAN_POINT('Ctrl Pts',(97.1281839866272,-0.011737821428815,1.77624707729253));
#8293=CARTESIAN_POINT('Ctrl Pts',(97.125130256148,0.0345399038578194,1.77625882609085));
#8294=CARTESIAN_POINT('Ctrl Pts',(97.1228720460036,0.069526154371763,1.77523376429706));
#8295=CARTESIAN_POINT('Ctrl Pts',(97.1165216538083,0.169246905730238,1.76935898348863));
#8296=CARTESIAN_POINT('Ctrl Pts',(97.1125149670027,0.233778716580485,1.7619944382235));
#8297=CARTESIAN_POINT('Ctrl Pts',(97.1004369633245,0.427498358375281,1.72905356259309));
#8298=CARTESIAN_POINT('Ctrl Pts',(97.0924259376233,0.554362751486858,1.69264849389071));
#8299=CARTESIAN_POINT('Ctrl Pts',(97.0822700322195,0.699969124711183,1.63272072156878));
#8300=CARTESIAN_POINT('Ctrl Pts',(97.0805852934568,0.723680343428494,1.62235026416194));
#8301=CARTESIAN_POINT('Ctrl Pts',(97.0779220324908,0.76041003395233,1.6053205562427));
#8302=CARTESIAN_POINT('Ctrl Pts',(97.0769555161355,0.773587780499568,1.59901201761015));
#8303=CARTESIAN_POINT('Ctrl Pts',(97.0751511134287,0.797898684095875,1.58700288557339));
#8304=CARTESIAN_POINT('Ctrl Pts',(97.0743147900584,0.809052416864327,1.58134583246737));
#8305=CARTESIAN_POINT('Ctrl Pts',(97.0724442750668,0.833739543536161,1.56849523935448));
#8306=CARTESIAN_POINT('Ctrl Pts',(97.0714080697921,0.847241306201684,1.56124344215834));
#8307=CARTESIAN_POINT('Ctrl Pts',(97.0683079974663,0.887108737226521,1.53916119616685));
#8308=CARTESIAN_POINT('Ctrl Pts',(97.0662265065759,0.913190054955769,1.5238316270869));
#8309=CARTESIAN_POINT('Ctrl Pts',(97.0562044215072,1.03546571249375,1.44769615303172));
#8310=CARTESIAN_POINT('Ctrl Pts',(97.0479601301718,1.12604724226921,1.37841333940808));
#8311=CARTESIAN_POINT('Ctrl Pts',(97.0323782557359,1.28212577806341,1.23332304985503));
#8312=CARTESIAN_POINT('Ctrl Pts',(97.0250919416703,1.34908743251226,1.15969768673858));
#8313=CARTESIAN_POINT('Ctrl Pts',(97.0168788342668,1.42037881719271,1.06672630988367));
#8314=CARTESIAN_POINT('Ctrl Pts',(97.0156418849221,1.43099943706171,1.05243606747396));
#8315=CARTESIAN_POINT('Ctrl Pts',(97.0138169933292,1.44651778841764,1.03088647885204));
#8316=CARTESIAN_POINT('Ctrl Pts',(97.0132188898722,1.45157926711454,1.02374717773884));
#8317=CARTESIAN_POINT('Ctrl Pts',(97.0121449304965,1.46062657865936,1.01078378399968));
#8318=CARTESIAN_POINT('Ctrl Pts',(97.0116678981872,1.46463066042491,1.00497308068935));
#8319=CARTESIAN_POINT('Ctrl Pts',(97.0105897675122,1.47364630178632,0.991721288962956));
#8320=CARTESIAN_POINT('Ctrl Pts',(97.0099900943235,1.47863623981172,0.984265927850673));
#8321=CARTESIAN_POINT('Ctrl Pts',(97.0081337285318,1.49399686650572,0.960935469534442));
#8322=CARTESIAN_POINT('Ctrl Pts',(97.0068891734624,1.50417036529532,0.944931318520012));
#8323=CARTESIAN_POINT('Ctrl Pts',(97.0039470835018,1.52785504372839,0.906320277871069));
#8324=CARTESIAN_POINT('Ctrl Pts',(97.0022618315973,1.54112385274543,0.883569406638891));
#8325=CARTESIAN_POINT('Ctrl Pts',(96.9956516835887,1.59170198507842,0.792239171381185));
#8326=CARTESIAN_POINT('Ctrl Pts',(96.9908701435527,1.62498086707824,0.721524026948818));
#8327=CARTESIAN_POINT('Ctrl Pts',(96.9792057480504,1.69440022418173,0.544617334105543));
#8328=CARTESIAN_POINT('Ctrl Pts',(96.9723253309013,1.72534918452841,0.436768439586762));
#8329=CARTESIAN_POINT('Ctrl Pts',(96.9635364352556,1.7504446312907,0.302666490877937));
#8330=CARTESIAN_POINT('Ctrl Pts',(96.9619454414689,1.75444970953147,0.278513079530205));
#8331=CARTESIAN_POINT('Ctrl Pts',(96.9593180936436,1.76018117208739,0.238889711297656));
#8332=CARTESIAN_POINT('Ctrl Pts',(96.9582911045482,1.76220574555847,0.223465740910955));
#8333=CARTESIAN_POINT('Ctrl Pts',(96.9564260201053,1.76549357143071,0.195584369913954));
#8334=CARTESIAN_POINT('Ctrl Pts',(96.9555902330909,1.76682819712699,0.183136300473857));
#8335=CARTESIAN_POINT('Ctrl Pts',(96.9537820195819,1.76941772206497,0.156311346428569));
#8336=CARTESIAN_POINT('Ctrl Pts',(96.9528082881519,1.77062921095662,0.141931279292703));
#8337=CARTESIAN_POINT('Ctrl Pts',(96.9500821747846,1.77351357510641,0.101863914718327));
#8338=CARTESIAN_POINT('Ctrl Pts',(96.9483179980546,1.77480341953332,0.0761535232723153));
#8339=CARTESIAN_POINT('Ctrl Pts',(96.9442757851557,1.77646166416109,0.0177647976588811));
#8340=CARTESIAN_POINT('Ctrl Pts',(96.9419887518329,1.77648754821479,-0.0149035008449363));
#8341=CARTESIAN_POINT('Ctrl Pts',(96.9396785508644,1.77561363580749,-0.0475423898693833));
#8342=CARTESIAN_POINT('',(96.9801888256167,-0.00138251417933347,1.77624916100617));
#8343=CARTESIAN_POINT('Ctrl Pts',(96.7921246218182,1.77561363837209,-0.0475422940869062));
#8344=CARTESIAN_POINT('Ctrl Pts',(96.7922437685583,1.77566277130408,-0.0457072731687558));
#8345=CARTESIAN_POINT('Ctrl Pts',(96.7923627957961,1.7757090601137,-0.0438721573609598));
#8346=CARTESIAN_POINT('Ctrl Pts',(96.7943923145719,1.7764505530197,-0.0125495285269162));
#8347=CARTESIAN_POINT('Ctrl Pts',(96.7962722099045,1.77641404750837,0.0169523811319034));
#8348=CARTESIAN_POINT('Ctrl Pts',(96.8042962371452,1.77308574138958,0.144207381436421));
#8349=CARTESIAN_POINT('Ctrl Pts',(96.8102291969789,1.76245856168471,0.241600729689548));
#8350=CARTESIAN_POINT('Ctrl Pts',(96.8221323450874,1.72571382706155,0.431388848441539));
#8351=CARTESIAN_POINT('Ctrl Pts',(96.8280805935747,1.70003152890578,0.523520821034303));
#8352=CARTESIAN_POINT('Ctrl Pts',(96.8357144305895,1.65939582986076,0.634006342816208));
#8353=CARTESIAN_POINT('Ctrl Pts',(96.8371683455194,1.65132886099307,0.654730084574135));
#8354=CARTESIAN_POINT('Ctrl Pts',(96.8395389566912,1.63766687352809,0.687967264574194));
#8355=CARTESIAN_POINT('Ctrl Pts',(96.8404475313342,1.63231219870343,0.700577343294984));
#8356=CARTESIAN_POINT('Ctrl Pts',(96.8422056839233,1.62172756777363,0.72472350822251));
#8357=CARTESIAN_POINT('Ctrl Pts',(96.8430544860503,1.6165190168332,0.736268104208643));
#8358=CARTESIAN_POINT('Ctrl Pts',(96.8450435034146,1.60408831789244,0.76305250186109));
#8359=CARTESIAN_POINT('Ctrl Pts',(96.8461869253768,1.59677180622489,0.778246886761163));
#8360=CARTESIAN_POINT('Ctrl Pts',(96.8500020979588,1.5718059326399,0.828259560446652));
#8361=CARTESIAN_POINT('Ctrl Pts',(96.852705836114,1.55322634147074,0.862597999351462));
#8362=CARTESIAN_POINT('Ctrl Pts',(96.8594521292481,1.5047419045311,0.945553372479553));
#8363=CARTESIAN_POINT('Ctrl Pts',(96.8635332741876,1.47359766824722,0.993392295439538));
#8364=CARTESIAN_POINT('Ctrl Pts',(96.8705574053086,1.41680746957138,1.07206301221505));
#8365=CARTESIAN_POINT('Ctrl Pts',(96.8734732699792,1.39231952950349,1.10367960218034));
#8366=CARTESIAN_POINT('Ctrl Pts',(96.8839312565245,1.30094814819622,1.21376468954196));
#8367=CARTESIAN_POINT('Ctrl Pts',(96.8915029359685,1.22832426597517,1.28721164200949));
#8368=CARTESIAN_POINT('Ctrl Pts',(96.8999669219529,1.13627161330593,1.36538009295072));
#8369=CARTESIAN_POINT('Ctrl Pts',(96.9011938045346,1.12263901421325,1.3766109400705));
#8370=CARTESIAN_POINT('Ctrl Pts',(96.9030068711349,1.10202560449784,1.39308281473312));
#8371=CARTESIAN_POINT('Ctrl Pts',(96.9036030331115,1.09517046134036,1.39847839824765));
#8372=CARTESIAN_POINT('Ctrl Pts',(96.9046750712617,1.08269809366977,1.40814725988875));
#8373=CARTESIAN_POINT('Ctrl Pts',(96.9051521007454,1.07709490636209,1.41243776295829));
#8374=CARTESIAN_POINT('Ctrl Pts',(96.9062321733752,1.06428748731943,1.42212419060212));
#8375=CARTESIAN_POINT('Ctrl Pts',(96.9068337668854,1.05706764996443,1.4274988831171));
#8376=CARTESIAN_POINT('Ctrl Pts',(96.9087025582789,1.03438200029868,1.44412035593852));
#8377=CARTESIAN_POINT('Ctrl Pts',(96.9099573847161,1.01877465662034,1.4551728407666));
#8378=CARTESIAN_POINT('Ctrl Pts',(96.91292866658,0.981009434937713,1.48101111751221));
#8379=CARTESIAN_POINT('Ctrl Pts',(96.9146325083126,0.958691101456287,1.49555506853468));
#8380=CARTESIAN_POINT('Ctrl Pts',(96.9229139142508,0.847481151165387,1.56451302829528));
#8381=CARTESIAN_POINT('Ctrl Pts',(96.9292263006332,0.754241933742447,1.61153574269311));
#8382=CARTESIAN_POINT('Ctrl Pts',(96.9410682152184,0.575638153710478,1.68269222118986));
#8383=CARTESIAN_POINT('Ctrl Pts',(96.9465494071981,0.491564871815255,1.70914417241013));
#8384=CARTESIAN_POINT('Ctrl Pts',(96.9538614853282,0.381286077192493,1.73502834236508));
#8385=CARTESIAN_POINT('Ctrl Pts',(96.9555073811031,0.35656946099771,1.74027599454798));
#8386=CARTESIAN_POINT('Ctrl Pts',(96.9581226318639,0.317527721943207,1.74769842969621));
#8387=CARTESIAN_POINT('Ctrl Pts',(96.9590806950033,0.303272988465862,1.75022830766665));
#8388=CARTESIAN_POINT('Ctrl Pts',(96.9608773366331,0.276641223220803,1.75461970698126));
#8389=CARTESIAN_POINT('Ctrl Pts',(96.961714459652,0.26427228374705,1.75652521436954));
#8390=CARTESIAN_POINT('Ctrl Pts',(96.9633643921041,0.239977636233082,1.76000553399761));
#8391=CARTESIAN_POINT('Ctrl Pts',(96.964176839764,0.228054007247566,1.76159021992694));
#8392=CARTESIAN_POINT('Ctrl Pts',(96.9660239477529,0.201039240146856,1.76490169526194));
#8393=CARTESIAN_POINT('Ctrl Pts',(96.9670608165743,0.185940365010559,1.76655623337296));
#8394=CARTESIAN_POINT('Ctrl Pts',(96.9720524385833,0.113580530829335,1.77354750697522));
#8395=CARTESIAN_POINT('Ctrl Pts',(96.9760859240408,0.0561108169463007,1.77629428175891));
#8396=CARTESIAN_POINT('Ctrl Pts',(96.9801884594846,-0.00138470182539974,
1.77624946026758));
#8397=CARTESIAN_POINT('Ctrl Pts',(96.9801883060489,-0.00138255147987768,
1.77624946194261));
#8398=CARTESIAN_POINT('Ctrl Pts',(96.9888781118596,-0.123167018364227,1.77615467047411));
#8399=CARTESIAN_POINT('Ctrl Pts',(96.9978703122374,-0.244618001788385,1.76353484642063));
#8400=CARTESIAN_POINT('Ctrl Pts',(97.0096401642456,-0.403294066310954,1.73033093233982));
#8401=CARTESIAN_POINT('Ctrl Pts',(97.0125459753947,-0.442486778458538,1.72072574469952));
#8402=CARTESIAN_POINT('Ctrl Pts',(97.0172282731229,-0.506103334100098,1.70281717563903));
#8403=CARTESIAN_POINT('Ctrl Pts',(97.0190323767654,-0.530733068229441,1.6953021845568));
#8404=CARTESIAN_POINT('Ctrl Pts',(97.021506568238,-0.564785934503054,1.68409706251978));
#8405=CARTESIAN_POINT('Ctrl Pts',(97.0221994295379,-0.574352860200603,1.68085837357009));
#8406=CARTESIAN_POINT('Ctrl Pts',(97.0233762264753,-0.590663598176203,1.67518118042147));
#8407=CARTESIAN_POINT('Ctrl Pts',(97.0238624382114,-0.597421114109849,1.67278315795344));
#8408=CARTESIAN_POINT('Ctrl Pts',(97.0248867384612,-0.611699108923349,1.66761880065494));
#8409=CARTESIAN_POINT('Ctrl Pts',(97.0254242396394,-0.619215623776566,1.66484241949637));
#8410=CARTESIAN_POINT('Ctrl Pts',(97.026905113785,-0.639982151907685,1.65701176974645));
#8411=CARTESIAN_POINT('Ctrl Pts',(97.0278423776131,-0.653191150663329,1.65184942168224));
#8412=CARTESIAN_POINT('Ctrl Pts',(97.0345283700719,-0.747756006590991,1.61357976904493));
#8413=CARTESIAN_POINT('Ctrl Pts',(97.0399796584938,-0.826629830325608,1.57463199548102));
#8414=CARTESIAN_POINT('Ctrl Pts',(97.0496472008356,-0.961930678130402,1.49483943245545));
#8415=CARTESIAN_POINT('Ctrl Pts',(97.0538715129715,-1.0194478007896,1.4562216898493));
#8416=CARTESIAN_POINT('Ctrl Pts',(97.0613941257715,-1.11613280631746,1.38276425876093));
#8417=CARTESIAN_POINT('Ctrl Pts',(97.0646604321251,-1.15628620920349,1.34936690664802));
#8418=CARTESIAN_POINT('Ctrl Pts',(97.0696072688698,-1.21370096103492,1.2971657998148));
#8419=CARTESIAN_POINT('Ctrl Pts',(97.071240153233,-1.23212383489966,1.27967960588984));
#8420=CARTESIAN_POINT('Ctrl Pts',(97.0742507054329,-1.26506335087017,1.24704395982025));
#8421=CARTESIAN_POINT('Ctrl Pts',(97.0756230273378,-1.27969875370991,1.23202068102459));
#8422=CARTESIAN_POINT('Ctrl Pts',(97.0770514721577,-1.29452735232963,1.21624974970036));
#8423=CARTESIAN_POINT('Ctrl Pts',(97.0770960959958,-1.2949901852817,1.2157569410033));
#8424=CARTESIAN_POINT('Ctrl Pts',(97.0771851926868,-1.29591347729013,1.21477272581397));
#8425=CARTESIAN_POINT('Ctrl Pts',(97.0772296654398,-1.2963739384717,1.21428132146262));
#8426=CARTESIAN_POINT('Ctrl Pts',(97.0773189916011,-1.29729799520658,1.21329404306859));
#8427=CARTESIAN_POINT('Ctrl Pts',(97.0773638451912,-1.29776158616472,1.21279816490042));
#8428=CARTESIAN_POINT('Ctrl Pts',(97.0774545117024,-1.29869785782136,1.21179553424503));
#8429=CARTESIAN_POINT('Ctrl Pts',(97.0775003251194,-1.29917052643283,1.21128877067853));
#8430=CARTESIAN_POINT('Ctrl Pts',(97.0783710958697,-1.3081463941225,1.2016541500088));
#8431=CARTESIAN_POINT('Ctrl Pts',(97.0792000631972,-1.31655330769046,1.19243744455801));
#8432=CARTESIAN_POINT('Ctrl Pts',(97.080884849684,-1.33335661767487,1.17362124341324));
#8433=CARTESIAN_POINT('Ctrl Pts',(97.0817408050526,-1.34174809092055,1.16401835839392));
#8434=CARTESIAN_POINT('Ctrl Pts',(97.0836346313891,-1.35999131981821,1.14268209929668));
#8435=CARTESIAN_POINT('Ctrl Pts',(97.0846743446301,-1.36979604571571,1.13091004835098));
#8436=CARTESIAN_POINT('Ctrl Pts',(97.0882567343631,-1.40285218236564,1.09016057494093));
#8437=CARTESIAN_POINT('Ctrl Pts',(97.0908289821726,-1.42534474758043,1.06058300888247));
#8438=CARTESIAN_POINT('Ctrl Pts',(97.1025801316417,-1.52252384841471,0.92411361179058));
#8439=CARTESIAN_POINT('Ctrl Pts',(97.1121417022289,-1.58622164205634,0.809911189767498));
#8440=CARTESIAN_POINT('Ctrl Pts',(97.1268676280928,-1.66456113263312,0.624015341245022));
#8441=CARTESIAN_POINT('Ctrl Pts',(97.1320419515988,-1.688293013959,0.556621562040473));
#8442=CARTESIAN_POINT('Ctrl Pts',(97.1382798557681,-1.71274574132034,0.471037620343215));
#8443=CARTESIAN_POINT('Ctrl Pts',(97.1395035918621,-1.71733344477497,0.454026774933829));
#8444=CARTESIAN_POINT('Ctrl Pts',(97.1413129643585,-1.72381133309032,0.428502624925536));
#8445=CARTESIAN_POINT('Ctrl Pts',(97.1419085216915,-1.72589301759252,0.420039654730272));
#8446=CARTESIAN_POINT('Ctrl Pts',(97.1429321472193,-1.72938451851909,0.405380829924952));
#8447=CARTESIAN_POINT('Ctrl Pts',(97.1433618216244,-1.73082346667513,0.399192385694116));
#8448=CARTESIAN_POINT('Ctrl Pts',(97.1443713483996,-1.73414105584454,0.384569273484682));
#8449=CARTESIAN_POINT('Ctrl Pts',(97.1449495970272,-1.73599139291627,0.376128461029571));
#8450=CARTESIAN_POINT('Ctrl Pts',(97.1466360808566,-1.74123765446337,0.351332466613573));
#8451=CARTESIAN_POINT('Ctrl Pts',(97.1477353559214,-1.74446467080607,0.334941984876958));
#8452=CARTESIAN_POINT('Ctrl Pts',(97.1562366591382,-1.7678494486457,0.206643778443689));
#8453=CARTESIAN_POINT('Ctrl Pts',(97.1631620696565,-1.77745305689395,0.0930646441787165));
#8454=CARTESIAN_POINT('Ctrl Pts',(97.1719650990916,-1.77578481163069,-0.0503142245878193));
#8455=CARTESIAN_POINT('Ctrl Pts',(97.1737870088823,-1.77469752648212,-0.0799491757074712));
#8456=CARTESIAN_POINT('Ctrl Pts',(97.1791756440195,-1.76931604337451,-0.167044589364597));
#8457=CARTESIAN_POINT('Ctrl Pts',(97.182765326705,-1.76296786597526,-0.224336213576346));
#8458=CARTESIAN_POINT('Ctrl Pts',(97.1889273187664,-1.74762663853319,-0.320014534657242));
#8459=CARTESIAN_POINT('Ctrl Pts',(97.1914582004671,-1.74012006453733,-0.358594435874066));
#8460=CARTESIAN_POINT('Ctrl Pts',(97.1951352568546,-1.72756346416243,-0.413369483262266));
#8461=CARTESIAN_POINT('Ctrl Pts',(97.1962485782657,-1.72355114409207,-0.42979212814451));
#8462=CARTESIAN_POINT('Ctrl Pts',(97.19820960432,-1.71612243011675,-0.458419486717947));
#8463=CARTESIAN_POINT('Ctrl Pts',(97.1990539469004,-1.71280863784795,-0.47064973898909));
#8464=CARTESIAN_POINT('Ctrl Pts',(97.200818942107,-1.70564502230207,-0.496010411814038));
#8465=CARTESIAN_POINT('Ctrl Pts',(97.2017402443821,-1.70177377224475,-0.509133853307769));
#8466=CARTESIAN_POINT('Ctrl Pts',(97.204166455181,-1.69123798005035,-0.543386593288768));
#8467=CARTESIAN_POINT('Ctrl Pts',(97.2056792521123,-1.6843292329152,-0.564437642741746));
#8468=CARTESIAN_POINT('Ctrl Pts',(97.2135102461873,-1.64685447371526,-0.671802316721369));
#8469=CARTESIAN_POINT('Ctrl Pts',(97.2200321965358,-1.61004561045119,-0.755775409602791));
#8470=CARTESIAN_POINT('Ctrl Pts',(97.2325340341959,-1.52892464780371,-0.907726680286481));
#8471=CARTESIAN_POINT('Ctrl Pts',(97.2384701622505,-1.48610618988684,-0.976251142072641));
#8472=CARTESIAN_POINT('Ctrl Pts',(97.2474109210745,-1.41397264494414,-1.07588781732506));
#8473=CARTESIAN_POINT('Ctrl Pts',(97.2504623162311,-1.38795042163254,-1.10925529229559));
#8474=CARTESIAN_POINT('Ctrl Pts',(97.2553484521581,-1.34366570940094,-1.16203867603485));
#8475=CARTESIAN_POINT('Ctrl Pts',(97.2572136041881,-1.32611467559119,-1.18202854208054));
#8476=CARTESIAN_POINT('Ctrl Pts',(97.2597559673009,-1.301203641617,-1.2091475009338));
#8477=CARTESIAN_POINT('Ctrl Pts',(97.2604575706657,-1.29422199103556,-1.2166174610547));
#8478=CARTESIAN_POINT('Ctrl Pts',(97.2616444642072,-1.28222137046485,-1.22923720861687));
#8479=CARTESIAN_POINT('Ctrl Pts',(97.2621321309166,-1.27723499451919,-1.23441748790563));
#8480=CARTESIAN_POINT('Ctrl Pts',(97.2631542330905,-1.26666422153393,-1.24526668877775));
#8481=CARTESIAN_POINT('Ctrl Pts',(97.2636881355722,-1.26107301145638,-1.25092855202763));
#8482=CARTESIAN_POINT('Ctrl Pts',(97.2651483664758,-1.24559575493238,-1.26639214894037));
#8483=CARTESIAN_POINT('Ctrl Pts',(97.2660688617533,-1.23563199304419,-1.27611577341478));
#8484=CARTESIAN_POINT('Ctrl Pts',(97.2716269416035,-1.17428053351596,-1.33459620959885));
#8485=CARTESIAN_POINT('Ctrl Pts',(97.2760727785378,-1.12012235394852,-1.38036593561045));
#8486=CARTESIAN_POINT('Ctrl Pts',(97.2873208262136,-0.974572906350596,-1.48914765574475));
#8487=CARTESIAN_POINT('Ctrl Pts',(97.2940236613079,-0.879761440665309,-1.54705296543348));
#8488=CARTESIAN_POINT('Ctrl Pts',(97.3034050939055,-0.745253040993197,-1.61281514062893));
#8489=CARTESIAN_POINT('Ctrl Pts',(97.3058657814968,-0.709785986780823,-1.62873519338897));
#8490=CARTESIAN_POINT('Ctrl Pts',(97.3102654868022,-0.646408509465607,-1.65471999003766));
#8491=CARTESIAN_POINT('Ctrl Pts',(97.3121887995141,-0.618714421747461,-1.66527310285286));
#8492=CARTESIAN_POINT('Ctrl Pts',(97.3151337692743,-0.576429123368358,-1.68018593816973));
#8493=CARTESIAN_POINT('Ctrl Pts',(97.3161384504943,-0.56202370540974,-1.68505924275226));
#8494=CARTESIAN_POINT('Ctrl Pts',(97.3178994086071,-0.536822030139404,-1.69322577682258));
#8495=CARTESIAN_POINT('Ctrl Pts',(97.3186528952439,-0.526053510895679,-1.69660222707012));
#8496=CARTESIAN_POINT('Ctrl Pts',(97.320365299605,-0.501619438624628,-1.70400850216787));
#8497=CARTESIAN_POINT('Ctrl Pts',(97.321326168154,-0.487936249435783,-1.70797694144979));
#8498=CARTESIAN_POINT('Ctrl Pts',(97.3239343656804,-0.45087785510985,-1.71824306951903));
#8499=CARTESIAN_POINT('Ctrl Pts',(97.3255916367632,-0.427419947876987,-1.7242279934651));
#8500=CARTESIAN_POINT('Ctrl Pts',(97.3373022631047,-0.262357853849691,-1.76276576962774));
#8501=CARTESIAN_POINT('Ctrl Pts',(97.3479074822279,-0.117373005340089,-1.77830885307717));
#8502=CARTESIAN_POINT('Ctrl Pts',(97.3627151341032,0.0852418244054738,-1.77513171131178));
#8503=CARTESIAN_POINT('Ctrl Pts',(97.3668934723986,0.142560325561041,-1.77145027518955));
#8504=CARTESIAN_POINT('Ctrl Pts',(97.3733052064261,0.231865169953898,-1.76135083838498));
#8505=CARTESIAN_POINT('Ctrl Pts',(97.3755935924289,0.264023904640286,-1.75681812560288));
#8506=CARTESIAN_POINT('Ctrl Pts',(97.3786008775865,0.306884651916257,-1.74957331436839));
#8507=CARTESIAN_POINT('Ctrl Pts',(97.3793567387839,0.317709837809064,-1.74763996476218));
#8508=CARTESIAN_POINT('Ctrl Pts',(97.3806074259483,0.335720762319991,-1.74425037442664));
#8509=CARTESIAN_POINT('Ctrl Pts',(97.3811052574871,0.342916576746842,-1.74284997277102));
#8510=CARTESIAN_POINT('Ctrl Pts',(97.3821192954709,0.357632504092766,-1.73989138378944));
#8511=CARTESIAN_POINT('Ctrl Pts',(97.3826352604509,0.365151520437643,-1.73832891252584));
#8512=CARTESIAN_POINT('Ctrl Pts',(97.3839933204874,0.385016872022323,-1.73406625726528));
#8513=CARTESIAN_POINT('Ctrl Pts',(97.3848308694473,0.397345189167589,-1.73128293460842));
#8514=CARTESIAN_POINT('Ctrl Pts',(97.3885834959496,0.452867912009762,-1.71812340914117));
#8515=CARTESIAN_POINT('Ctrl Pts',(97.391425062721,0.495697129025543,-1.70625978845645));
#8516=CARTESIAN_POINT('Ctrl Pts',(97.4026489644181,0.665622795597073,-1.65225061430707));
#8517=CARTESIAN_POINT('Ctrl Pts',(97.4106630685918,0.788216230640514,-1.59740565909893));
#8518=CARTESIAN_POINT('Ctrl Pts',(97.4229383930489,0.957407710078322,-1.49744998751428));
#8519=CARTESIAN_POINT('Ctrl Pts',(97.4269119345481,1.00959894993034,-1.4627695270249));
#8520=CARTESIAN_POINT('Ctrl Pts',(97.4322776110068,1.07575223229045,-1.41358199429229));
#8521=CARTESIAN_POINT('Ctrl Pts',(97.4335773439042,1.09145831242276,-1.40149049955702));
#8522=CARTESIAN_POINT('Ctrl Pts',(97.4357598612371,1.11728101885328,-1.38091325260486));
#8523=CARTESIAN_POINT('Ctrl Pts',(97.4366368308502,1.12751151318121,-1.37257278785242));
#8524=CARTESIAN_POINT('Ctrl Pts',(97.4383719095569,1.14746096314669,-1.35593535014906));
#8525=CARTESIAN_POINT('Ctrl Pts',(97.4392296757877,1.15718522786088,-1.34764597329514));
#8526=CARTESIAN_POINT('Ctrl Pts',(97.441132413044,1.17844747446322,-1.32912131747619));
#8527=CARTESIAN_POINT('Ctrl Pts',(97.4421792919348,1.18994317513302,-1.31883931559493));
#8528=CARTESIAN_POINT('Ctrl Pts',(97.4452915682999,1.22351445935931,-1.28801616653578));
#8529=CARTESIAN_POINT('Ctrl Pts',(97.447374251714,1.24520156455222,-1.26706201476719));
#8530=CARTESIAN_POINT('Ctrl Pts',(97.4589226506963,1.36118556753658,-1.14914334412415));
#8531=CARTESIAN_POINT('Ctrl Pts',(97.4688289373423,1.44469092034567,-1.04221556110278));
#8532=CARTESIAN_POINT('Ctrl Pts',(97.4840305025927,1.55331995211775,-0.864630232680956));
#8533=CARTESIAN_POINT('Ctrl Pts',(97.4893244391102,1.58752763775887,-0.800091461380455));
#8534=CARTESIAN_POINT('Ctrl Pts',(97.4956875000583,1.62501741712128,-0.717425181961458));
#8535=CARTESIAN_POINT('Ctrl Pts',(97.4969234379416,1.63212104036389,-0.70111444685532));
#8536=CARTESIAN_POINT('Ctrl Pts',(97.4987471300399,1.64235095052128,-0.676626890032803));
#8537=CARTESIAN_POINT('Ctrl Pts',(97.4993450271165,1.64566355765598,-0.668529772071085));
#8538=CARTESIAN_POINT('Ctrl Pts',(97.5003711068295,1.65127908927038,-0.654508837426563));
#8539=CARTESIAN_POINT('Ctrl Pts',(97.5008009218634,1.65361018774981,-0.648596792651734));
#8540=CARTESIAN_POINT('Ctrl Pts',(97.5018085270933,1.6590246788308,-0.634645808050767));
#8541=CARTESIAN_POINT('Ctrl Pts',(97.5023847395692,1.6620814147094,-0.626596812349615));
#8542=CARTESIAN_POINT('Ctrl Pts',(97.5040594036382,1.67084406726151,-0.603007632693148));
#8543=CARTESIAN_POINT('Ctrl Pts',(97.5051490821601,1.67639158786321,-0.58740905220074));
#8544=CARTESIAN_POINT('Ctrl Pts',(97.5137502702867,1.71884952684422,-0.462521744043253));
#8545=CARTESIAN_POINT('Ctrl Pts',(97.5207697033183,1.74525699913278,-0.349936298998502));
#8546=CARTESIAN_POINT('Ctrl Pts',(97.5317197955851,1.76890942707055,-0.173168709070312));
#8547=CARTESIAN_POINT('Ctrl Pts',(97.5355920537966,1.77393052506702,-0.110403668282001));
#8548=CARTESIAN_POINT('Ctrl Pts',(97.5395353031289,1.77561364475627,-0.0475420556493824));
#8549=CARTESIAN_POINT('Origin',(88.3562164250559,0.,0.));
#8550=CARTESIAN_POINT('',(98.436744300164,1.7756136383717,-0.047542294101169));
#8551=CARTESIAN_POINT('',(98.2893138640945,1.77561363880419,-0.0475422779488097));
#8552=CARTESIAN_POINT('',(88.3562164250559,1.77561363837197,-0.0475422940912398));
#8553=CARTESIAN_POINT('',(97.8793796642132,0.00163535216639757,1.77624916181758));
#8554=CARTESIAN_POINT('Ctrl Pts',(98.436744300164,1.7756136383717,-0.047542294101169));
#8555=CARTESIAN_POINT('Ctrl Pts',(98.4364498240271,1.77549319424063,-0.0520406517400838));
#8556=CARTESIAN_POINT('Ctrl Pts',(98.4361561234276,1.77535565357106,-0.0565386361140695));
#8557=CARTESIAN_POINT('Ctrl Pts',(98.4311977724099,1.77273844685076,-0.132658575839666));
#8558=CARTESIAN_POINT('Ctrl Pts',(98.4267239300063,1.76594329645432,-0.20407454630018));
#8559=CARTESIAN_POINT('Ctrl Pts',(98.4141953155081,1.73453508085451,-0.404578135937726));
#8560=CARTESIAN_POINT('Ctrl Pts',(98.4062659760535,1.69990889600267,-0.531604606724482));
#8561=CARTESIAN_POINT('Ctrl Pts',(98.3955350445561,1.63793764026522,-0.688188708671686));
#8562=CARTESIAN_POINT('Ctrl Pts',(98.3931391781615,1.62319149197298,-0.722282827827224));
#8563=CARTESIAN_POINT('Ctrl Pts',(98.3896351500677,1.60041890180874,-0.770708521507362));
#8564=CARTESIAN_POINT('Ctrl Pts',(98.3885560132639,1.59324495485693,-0.785431582274868));
#8565=CARTESIAN_POINT('Ctrl Pts',(98.3866316427076,1.58017679376829,-0.811335351670994));
#8566=CARTESIAN_POINT('Ctrl Pts',(98.3857893296536,1.57436483616474,-0.822556442399754));
#8567=CARTESIAN_POINT('Ctrl Pts',(98.3840189450417,1.56196142527674,-0.845890488638317));
#8568=CARTESIAN_POINT('Ctrl Pts',(98.3830901233183,1.55534767344118,-0.857990564550234));
#8569=CARTESIAN_POINT('Ctrl Pts',(98.3806213227468,1.53749338176221,-0.889770635239372));
#8570=CARTESIAN_POINT('Ctrl Pts',(98.379072940221,1.52601623550939,-0.909314053726346));
#8571=CARTESIAN_POINT('Ctrl Pts',(98.3756282868196,1.49988411870613,-0.951923445489135));
#8572=CARTESIAN_POINT('Ctrl Pts',(98.3737264128007,1.48506464933855,-0.974881256111815));
#8573=CARTESIAN_POINT('Ctrl Pts',(98.3676896827283,1.43681408146994,-1.04597483981874));
#8574=CARTESIAN_POINT('Ctrl Pts',(98.363493518691,1.4015295071744,-1.09280007310644));
#8575=CARTESIAN_POINT('Ctrl Pts',(98.3510962686073,1.29193994017567,-1.22417728151325));
#8576=CARTESIAN_POINT('Ctrl Pts',(98.3427739988167,1.21183999426396,-1.30351922822059));
#8577=CARTESIAN_POINT('Ctrl Pts',(98.3319802823211,1.09535447533574,-1.39882365770442));
#8578=CARTESIAN_POINT('Ctrl Pts',(98.329287957368,1.0651661475218,-1.42194606282038));
#8579=CARTESIAN_POINT('Ctrl Pts',(98.3258215630699,1.02452613141695,-1.45105255546659));
#8580=CARTESIAN_POINT('Ctrl Pts',(98.3249972334819,1.01472508825768,-1.45792329280199));
#8581=CARTESIAN_POINT('Ctrl Pts',(98.3236643845982,0.998642196679764,-1.46895697412623));
#8582=CARTESIAN_POINT('Ctrl Pts',(98.3231520380507,0.992402177815162,-1.47317980968612));
#8583=CARTESIAN_POINT('Ctrl Pts',(98.3221389492554,0.979944398176783,-1.48149534039439));
#8584=CARTESIAN_POINT('Ctrl Pts',(98.3216381612921,0.973727428107289,-1.48558889579128));
#8585=CARTESIAN_POINT('Ctrl Pts',(98.3203670385265,0.957802482630964,-1.49593173566324));
#8586=CARTESIAN_POINT('Ctrl Pts',(98.319600249639,0.948058781504405,-1.50212579962672));
#8587=CARTESIAN_POINT('Ctrl Pts',(98.3163710769934,0.906478407406836,-1.52799263392985));
#8588=CARTESIAN_POINT('Ctrl Pts',(98.313961045111,0.874082307631577,-1.54675310553334));
#8589=CARTESIAN_POINT('Ctrl Pts',(98.3069674180164,0.776938001593733,-1.59898111633273));
#8590=CARTESIAN_POINT('Ctrl Pts',(98.3024911482823,0.7106941327705,-1.62950561828538));
#8591=CARTESIAN_POINT('Ctrl Pts',(98.2906967785278,0.53158988904329,-1.69902819980099));
#8592=CARTESIAN_POINT('Ctrl Pts',(98.2833946947551,0.416371093931519,-1.73087140908704));
#8593=CARTESIAN_POINT('Ctrl Pts',(98.2741449514429,0.274865870806526,-1.75502255525102));
#8594=CARTESIAN_POINT('Ctrl Pts',(98.2725643259572,0.250814224237256,-1.75862092273437));
#8595=CARTESIAN_POINT('Ctrl Pts',(98.2699505545576,0.211315506337741,-1.76370358420352));
#8596=CARTESIAN_POINT('Ctrl Pts',(98.2689266055335,0.195908989197235,-1.76548129942933));
#8597=CARTESIAN_POINT('Ctrl Pts',(98.267064742168,0.168030104502262,-1.76832875981146));
#8598=CARTESIAN_POINT('Ctrl Pts',(98.2662290992367,0.155565829647346,-1.76946884054118));
#8599=CARTESIAN_POINT('Ctrl Pts',(98.2644185886328,0.128671633307802,-1.77164244253615));
#8600=CARTESIAN_POINT('Ctrl Pts',(98.2634423871007,0.114239137391958,-1.77263158363403));
#8601=CARTESIAN_POINT('Ctrl Pts',(98.2607019125536,0.073924309156453,-1.77490020865661));
#8602=CARTESIAN_POINT('Ctrl Pts',(98.2589256410564,0.0480245868690461,-1.77578970311681));
#8603=CARTESIAN_POINT('Ctrl Pts',(98.2511907568331,-0.0637156155086965,
-1.7771810714908));
#8604=CARTESIAN_POINT('Ctrl Pts',(98.2450630746089,-0.149499456208484,-1.77202663779861));
#8605=CARTESIAN_POINT('Ctrl Pts',(98.2289914100532,-0.368907542626103,-1.74279653295528));
#8606=CARTESIAN_POINT('Ctrl Pts',(98.2189210969748,-0.500763045706761,-1.70958225491674));
#8607=CARTESIAN_POINT('Ctrl Pts',(98.2082251164003,-0.643639316351112,-1.65562310180338));
#8608=CARTESIAN_POINT('Ctrl Pts',(98.2070319525122,-0.65962883413529,-1.64931782283778));
#8609=CARTESIAN_POINT('Ctrl Pts',(98.2052585137159,-0.68350734298818,-1.63949878495326));
#8610=CARTESIAN_POINT('Ctrl Pts',(98.2046688648038,-0.691465830415999,-1.63615817297545));
#8611=CARTESIAN_POINT('Ctrl Pts',(98.2036511370002,-0.705240822678005,-1.6302575935744));
#8612=CARTESIAN_POINT('Ctrl Pts',(98.2032215203264,-0.711068238444655,-1.62772430183764));
#8613=CARTESIAN_POINT('Ctrl Pts',(98.2022064439018,-0.724866180770959,-1.6216378230353));
#8614=CARTESIAN_POINT('Ctrl Pts',(98.2016226562061,-0.73282426998406,-1.61805710853004));
#8615=CARTESIAN_POINT('Ctrl Pts',(98.199866499607,-0.756819732126975,-1.60704708427951));
#8616=CARTESIAN_POINT('Ctrl Pts',(98.1987044664364,-0.772773454218721,-1.59943667729234));
#8617=CARTESIAN_POINT('Ctrl Pts',(98.1928732159986,-0.853038453770335,-1.55966641513358));
#8618=CARTESIAN_POINT('Ctrl Pts',(98.1883853476541,-0.915474885686514,-1.52385758172097));
#8619=CARTESIAN_POINT('Ctrl Pts',(98.1757991777122,-1.08586835669961,-1.41186879055));
#8620=CARTESIAN_POINT('Ctrl Pts',(98.1678264465526,-1.18773237498556,-1.32731819330471));
#8621=CARTESIAN_POINT('Ctrl Pts',(98.1570861781658,-1.30458340611965,-1.20600805754049));
#8622=CARTESIAN_POINT('Ctrl Pts',(98.154733024162,-1.32906049843106,-1.17897887864473));
#8623=CARTESIAN_POINT('Ctrl Pts',(98.1512801076867,-1.3632290539861,-1.13883061183677));
#8624=CARTESIAN_POINT('Ctrl Pts',(98.1502081643678,-1.37359980289895,-1.12630021236477));
#8625=CARTESIAN_POINT('Ctrl Pts',(98.1482919914552,-1.39170965169996,-1.103796902547));
#8626=CARTESIAN_POINT('Ctrl Pts',(98.1474505962984,-1.39951736511529,-1.09388047214783));
#8627=CARTESIAN_POINT('Ctrl Pts',(98.1456773516888,-1.41566632264314,-1.07291406148234));
#8628=CARTESIAN_POINT('Ctrl Pts',(98.1447447018772,-1.42398534729773,-1.06184812104333));
#8629=CARTESIAN_POINT('Ctrl Pts',(98.1422541599318,-1.44573328471294,-1.03220385063352));
#8630=CARTESIAN_POINT('Ctrl Pts',(98.140687596042,-1.45893296429981,-1.01346141497995));
#8631=CARTESIAN_POINT('Ctrl Pts',(98.1309863637115,-1.53771799886348,-0.896863459877092));
#8632=CARTESIAN_POINT('Ctrl Pts',(98.122500698521,-1.59378544509857,-0.792956095033334));
#8633=CARTESIAN_POINT('Ctrl Pts',(98.1059342027565,-1.6811430969999,-0.583697823282789));
#8634=CARTESIAN_POINT('Ctrl Pts',(98.0979117060398,-1.71378990472506,-0.479450878684006));
#8635=CARTESIAN_POINT('Ctrl Pts',(98.0890734513185,-1.74028131645104,-0.356062133078072));
#8636=CARTESIAN_POINT('Ctrl Pts',(98.0878805388098,-1.74364440909747,-0.339210159587333));
#8637=CARTESIAN_POINT('Ctrl Pts',(98.0861073964421,-1.74832856695896,-0.313824415211005));
#8638=CARTESIAN_POINT('Ctrl Pts',(98.0855177970025,-1.74983272494863,-0.305326029302561));
#8639=CARTESIAN_POINT('Ctrl Pts',(98.0845001171586,-1.75233674593911,-0.290551834537751));
#8640=CARTESIAN_POINT('Ctrl Pts',(98.0840704995541,-1.7533649310515,-0.284281306837281));
#8641=CARTESIAN_POINT('Ctrl Pts',(98.0830553743316,-1.75572536987176,-0.269385685262963));
#8642=CARTESIAN_POINT('Ctrl Pts',(98.0824715393429,-1.7570277377871,-0.260756128408594));
#8643=CARTESIAN_POINT('Ctrl Pts',(98.0807150889001,-1.76077564968997,-0.234618163303082));
#8644=CARTESIAN_POINT('Ctrl Pts',(98.0795528142587,-1.76302355799085,-0.217081927580092));
#8645=CARTESIAN_POINT('Ctrl Pts',(98.0737190971453,-1.7730895312314,-0.128032963612148));
#8646=CARTESIAN_POINT('Ctrl Pts',(98.0692291743233,-1.77682072677008,-0.0561186120152204));
#8647=CARTESIAN_POINT('Ctrl Pts',(98.0566345562477,-1.77500221966316,0.147913529084895));
#8648=CARTESIAN_POINT('Ctrl Pts',(98.0486554499844,-1.75909658494166,0.279443545136796));
#8649=CARTESIAN_POINT('Ctrl Pts',(98.0379432557986,-1.72051310657633,0.442930355753527));
#8650=CARTESIAN_POINT('Ctrl Pts',(98.035626539613,-1.7112111265038,0.477607422824908));
#8651=CARTESIAN_POINT('Ctrl Pts',(98.0322015786947,-1.69613361538493,0.527697198407684));
#8652=CARTESIAN_POINT('Ctrl Pts',(98.0311199289867,-1.69118414416974,0.543350471583162));
#8653=CARTESIAN_POINT('Ctrl Pts',(98.0291926836041,-1.6820403441575,0.57093272406222));
#8654=CARTESIAN_POINT('Ctrl Pts',(98.0283500388017,-1.67793422260694,0.582889891159723));
#8655=CARTESIAN_POINT('Ctrl Pts',(98.0265805996596,-1.66908947021142,0.60777795701333));
#8656=CARTESIAN_POINT('Ctrl Pts',(98.0256530723141,-1.66432741053121,0.62069957028101));
#8657=CARTESIAN_POINT('Ctrl Pts',(98.0231916245013,-1.65136338049467,0.654654637687382));
#8658=CARTESIAN_POINT('Ctrl Pts',(98.0216493903083,-1.6429100585522,0.675588755524796));
#8659=CARTESIAN_POINT('Ctrl Pts',(98.0118529852273,-1.58717381741344,0.806378868563877));
#8660=CARTESIAN_POINT('Ctrl Pts',(98.0032349843248,-1.52930368236859,0.911366073932465));
#8661=CARTESIAN_POINT('Ctrl Pts',(97.9866284126233,-1.40010641559389,1.09834854595397));
#8662=CARTESIAN_POINT('Ctrl Pts',(97.9787037845345,-1.3309331086271,1.18122319923876));
#8663=CARTESIAN_POINT('Ctrl Pts',(97.9699474030927,-1.24244254822381,1.26952709552912));
#8664=CARTESIAN_POINT('Ctrl Pts',(97.968747840813,-1.23003552466186,1.28155187002866));
#8665=CARTESIAN_POINT('Ctrl Pts',(97.9669668709888,-1.21115693202138,1.29932203324005));
#8666=CARTESIAN_POINT('Ctrl Pts',(97.9663759760926,-1.20481602133872,1.30520390079967));
#8667=CARTESIAN_POINT('Ctrl Pts',(97.9653570469639,-1.19374275718619,1.31532606570448));
#8668=CARTESIAN_POINT('Ctrl Pts',(97.9649274601845,-1.18903037412981,1.31958751208561));
#8669=CARTESIAN_POINT('Ctrl Pts',(97.9639136364093,-1.17780528126715,1.32962949883111));
#8670=CARTESIAN_POINT('Ctrl Pts',(97.9633310568957,-1.17127281032193,1.33538754543905));
#8671=CARTESIAN_POINT('Ctrl Pts',(97.9617106378978,-1.15288177893972,1.35135953820233));
#8672=CARTESIAN_POINT('Ctrl Pts',(97.960680202148,-1.14092986342967,1.36146541832615));
#8673=CARTESIAN_POINT('Ctrl Pts',(97.9568232330882,-1.09529295588967,1.39903035090943));
#8674=CARTESIAN_POINT('Ctrl Pts',(97.9540592012098,-1.06073540648793,1.42540997514884));
#8675=CARTESIAN_POINT('Ctrl Pts',(97.9430159046634,-0.916900363792435,1.52707563437461));
#8676=CARTESIAN_POINT('Ctrl Pts',(97.9350664257595,-0.800318623036185,1.59127598507827));
#8677=CARTESIAN_POINT('Ctrl Pts',(97.9231224735167,-0.623983897376875,1.66405570736381));
#8678=CARTESIAN_POINT('Ctrl Pts',(97.9194302741321,-0.569247678466713,1.68356566639224));
#8679=CARTESIAN_POINT('Ctrl Pts',(97.9143575918865,-0.494637045618368,1.70610464833716));
#8680=CARTESIAN_POINT('Ctrl Pts',(97.913054707576,-0.475521620471654,1.71153089785536));
#8681=CARTESIAN_POINT('Ctrl Pts',(97.9109555654397,-0.444828751366333,1.71968974503466));
#8682=CARTESIAN_POINT('Ctrl Pts',(97.9101660200869,-0.433307562692562,1.72262879972795));
#8683=CARTESIAN_POINT('Ctrl Pts',(97.9085229511075,-0.409386056290628,1.72847601339143));
#8684=CARTESIAN_POINT('Ctrl Pts',(97.9076689232356,-0.39698226407884,1.73136689910523));
#8685=CARTESIAN_POINT('Ctrl Pts',(97.9059646715361,-0.372295530630285,1.73684127784819));
#8686=CARTESIAN_POINT('Ctrl Pts',(97.905114621494,-0.360014158679006,1.7394284630239));
#8687=CARTESIAN_POINT('Ctrl Pts',(97.9031159236725,-0.331217087005892,1.74517679465249));
#8688=CARTESIAN_POINT('Ctrl Pts',(97.9019640602107,-0.314682107919662,1.74823394900781));
#8689=CARTESIAN_POINT('Ctrl Pts',(97.8938788046602,-0.199066246213916,1.76791685285348));
#8690=CARTESIAN_POINT('Ctrl Pts',(97.8866915543347,-0.0987931240126965,
1.77634175479645));
#8691=CARTESIAN_POINT('Ctrl Pts',(97.8793797538287,0.00163615522257698,
1.7762492464449));
#8692=CARTESIAN_POINT('Ctrl Pts',(97.8793798115091,0.00163536296821643,
1.7762492471745));
#8693=CARTESIAN_POINT('Ctrl Pts',(97.8701489465145,0.12842344781845,1.77613251550573));
#8694=CARTESIAN_POINT('Ctrl Pts',(97.8607566791393,0.254844257215121,1.76244136402429));
#8695=CARTESIAN_POINT('Ctrl Pts',(97.8510352112,0.390526460359617,1.73282968049199));
#8696=CARTESIAN_POINT('Ctrl Pts',(97.8501958426688,0.402287510813218,1.73013710295976));
#8697=CARTESIAN_POINT('Ctrl Pts',(97.8486422596125,0.424157922583311,1.72489500807164));
#8698=CARTESIAN_POINT('Ctrl Pts',(97.8479265771266,0.434273992030345,1.72237593032756));
#8699=CARTESIAN_POINT('Ctrl Pts',(97.8467232858721,0.45136187029056,1.717960625396));
#8700=CARTESIAN_POINT('Ctrl Pts',(97.8462331385813,0.458345256861603,1.7161106845584));
#8701=CARTESIAN_POINT('Ctrl Pts',(97.8452139353772,0.472917549871457,1.71215509540286));
#8702=CARTESIAN_POINT('Ctrl Pts',(97.8446853299995,0.480504008581517,1.71004151512806));
#8703=CARTESIAN_POINT('Ctrl Pts',(97.8432554246691,0.501094868121651,1.70415706999478));
#8704=CARTESIAN_POINT('Ctrl Pts',(97.842359562017,0.514070918531787,1.70028777103803));
#8705=CARTESIAN_POINT('Ctrl Pts',(97.8375287995418,0.58436235787695,1.67844943302586));
#8706=CARTESIAN_POINT('Ctrl Pts',(97.8337307943092,0.640788414818756,1.65772845892284));
#8707=CARTESIAN_POINT('Ctrl Pts',(97.8239836348431,0.784851380338988,1.59636659444337));
#8708=CARTESIAN_POINT('Ctrl Pts',(97.8181365185447,0.870412805256262,1.55137374007192));
#8709=CARTESIAN_POINT('Ctrl Pts',(97.8072521675063,1.01883580541849,1.45716290885644));
#8710=CARTESIAN_POINT('Ctrl Pts',(97.802270518153,1.08284705075691,1.41024472440532));
#8711=CARTESIAN_POINT('Ctrl Pts',(97.7957629469704,1.15954461491003,1.34571900645595));
#8712=CARTESIAN_POINT('Ctrl Pts',(97.7943914964367,1.1753423755258,1.33194354159338));
#8713=CARTESIAN_POINT('Ctrl Pts',(97.7929663866391,1.19136624139158,1.31746383238738));
#8714=CARTESIAN_POINT('Ctrl Pts',(97.7929242128531,1.19184009107077,1.31703518103769));
#8715=CARTESIAN_POINT('Ctrl Pts',(97.7928395981406,1.19279008854765,1.31617486688233));
#8716=CARTESIAN_POINT('Ctrl Pts',(97.7927971570968,1.19326623356079,1.31574320115745));
#8717=CARTESIAN_POINT('Ctrl Pts',(97.7927115203567,1.1942262738616,1.31487189366832));
#8718=CARTESIAN_POINT('Ctrl Pts',(97.7926683242941,1.19471016088888,1.31443224298828));
#8719=CARTESIAN_POINT('Ctrl Pts',(97.7925806329629,1.19569174266412,1.31353940637621));
#8720=CARTESIAN_POINT('Ctrl Pts',(97.7925361370363,1.19618942272962,1.31308620452962));
#8721=CARTESIAN_POINT('Ctrl Pts',(97.7924452117151,1.19720561175954,1.31215977627235));
#8722=CARTESIAN_POINT('Ctrl Pts',(97.792398781297,1.19772409798665,1.31168652520156));
#8723=CARTESIAN_POINT('Ctrl Pts',(97.7923032176292,1.1987903794802,1.31071211172024));
#8724=CARTESIAN_POINT('Ctrl Pts',(97.7922540828689,1.19933814127114,1.31021091303418));
#8725=CARTESIAN_POINT('Ctrl Pts',(97.7921521396999,1.20047363373767,1.30917063564497));
#8726=CARTESIAN_POINT('Ctrl Pts',(97.7920993290948,1.2010613158117,1.30863150435542));
#8727=CARTESIAN_POINT('Ctrl Pts',(97.7919887602823,1.20229058906726,1.30750226072982));
#8728=CARTESIAN_POINT('Ctrl Pts',(97.7919309988614,1.20293210918085,1.30691207166756));
#8729=CARTESIAN_POINT('Ctrl Pts',(97.79180878787,1.20428804298039,1.30566278832957));
#8730=CARTESIAN_POINT('Ctrl Pts',(97.7917443334925,1.20500235040018,1.30500357961876));
#8731=CARTESIAN_POINT('Ctrl Pts',(97.7916062525742,1.20653086621023,1.30359064219827));
#8732=CARTESIAN_POINT('Ctrl Pts',(97.7915326185799,1.20734490983612,1.30283673659758));
#8733=CARTESIAN_POINT('Ctrl Pts',(97.7914017433997,1.20878987833227,1.30149599883434));
#8734=CARTESIAN_POINT('Ctrl Pts',(97.7913445150267,1.20942108419775,1.30090946880782));
#8735=CARTESIAN_POINT('Ctrl Pts',(97.7911442978448,1.21162715143311,1.29885655054649));
#8736=CARTESIAN_POINT('Ctrl Pts',(97.7910012072874,1.21319976965839,1.29738776463275));
#8737=CARTESIAN_POINT('Ctrl Pts',(97.7900254248622,1.22389661059604,1.28736072812023));
#8738=CARTESIAN_POINT('Ctrl Pts',(97.7891887641735,1.23293266851325,1.27870934102654));
#8739=CARTESIAN_POINT('Ctrl Pts',(97.7873129321521,1.25288548084041,1.2591978131394));
#8740=CARTESIAN_POINT('Ctrl Pts',(97.78627169125,1.26375379960836,1.24828981755339));
#8741=CARTESIAN_POINT('Ctrl Pts',(97.7835955445836,1.29115283437915,1.22006617252224));
#8742=CARTESIAN_POINT('Ctrl Pts',(97.7819519778819,1.3074773577559,1.20255559905682));
#8743=CARTESIAN_POINT('Ctrl Pts',(97.7696475394835,1.42594619136729,1.07021503337505));
#8744=CARTESIAN_POINT('Ctrl Pts',(97.758366896901,1.51313959683016,0.942906875832111));
#8745=CARTESIAN_POINT('Ctrl Pts',(97.7435743829219,1.60519890862316,0.762119559965586));
#8746=CARTESIAN_POINT('Ctrl Pts',(97.7400051867513,1.62571403238309,0.717317390210057));
#8747=CARTESIAN_POINT('Ctrl Pts',(97.7350692557899,1.65195559844421,0.653078976351917));
#8748=CARTESIAN_POINT('Ctrl Pts',(97.7336484304696,1.65925256249553,0.634311008894522));
#8749=CARTESIAN_POINT('Ctrl Pts',(97.7311604808452,1.67159626534977,0.600890964381311));
#8750=CARTESIAN_POINT('Ctrl Pts',(97.7300874769289,1.67677329432323,0.586289506784017));
#8751=CARTESIAN_POINT('Ctrl Pts',(97.7284562666619,1.6844261484165,0.563774165282989));
#8752=CARTESIAN_POINT('Ctrl Pts',(97.727890706222,1.68703855584239,0.555907975311019));
#8753=CARTESIAN_POINT('Ctrl Pts',(97.7268466064179,1.69178672199528,0.541269039885092));
#8754=CARTESIAN_POINT('Ctrl Pts',(97.7263672900859,1.69393698150973,0.534501628853972));
#8755=CARTESIAN_POINT('Ctrl Pts',(97.7252576935113,1.6988447916866,0.518728382762341));
#8756=CARTESIAN_POINT('Ctrl Pts',(97.7246291899807,1.70157137852542,0.509713267442633));
#8757=CARTESIAN_POINT('Ctrl Pts',(97.7225988897404,1.71019917986507,0.480345559955327));
#8758=CARTESIAN_POINT('Ctrl Pts',(97.7212125679938,1.71580817779871,0.45990812653986));
#8759=CARTESIAN_POINT('Ctrl Pts',(97.7114075839688,1.75330038296824,0.313049291815026));
#8760=CARTESIAN_POINT('Ctrl Pts',(97.7035642303021,1.77154816250142,0.183542283052406));
#8761=CARTESIAN_POINT('Ctrl Pts',(97.6934547137312,1.77645946109298,0.0196101616983407));
#8762=CARTESIAN_POINT('Ctrl Pts',(97.6913753020059,1.77651224263065,-0.0139812004696996));
#8763=CARTESIAN_POINT('Ctrl Pts',(97.6892780485025,1.77561363630377,-0.0475423713344133));
#8764=CARTESIAN_POINT('Ctrl Pts',(97.5395353031289,1.77561364475627,-0.0475420556493824));
#8765=CARTESIAN_POINT('Ctrl Pts',(97.5425586847016,1.77690413202303,0.000655414316051098));
#8766=CARTESIAN_POINT('Ctrl Pts',(97.5456233416066,1.77623234914152,0.0489096839338776));
#8767=CARTESIAN_POINT('Ctrl Pts',(97.5502625108346,1.77231499271284,0.120461303337754));
#8768=CARTESIAN_POINT('Ctrl Pts',(97.5517901044051,1.77057478767216,0.14379220025042));
#8769=CARTESIAN_POINT('Ctrl Pts',(97.5542510280419,1.76706288314405,0.18096195333014));
#8770=CARTESIAN_POINT('Ctrl Pts',(97.555175033585,1.76558801832578,0.194826569943365));
#8771=CARTESIAN_POINT('Ctrl Pts',(97.5569436102543,1.76247042131107,0.221180292731501));
#8772=CARTESIAN_POINT('Ctrl Pts',(97.5577871813323,1.76085775191497,0.233672144835478));
#8773=CARTESIAN_POINT('Ctrl Pts',(97.55971687325,1.7568851281505,0.262063040706086));
#8774=CARTESIAN_POINT('Ctrl Pts',(97.5608055638305,1.75444197532685,0.277949125473025));
#8775=CARTESIAN_POINT('Ctrl Pts',(97.5643084824895,1.74594203684482,0.328630141396153));
#8776=CARTESIAN_POINT('Ctrl Pts',(97.5667482812997,1.73906331039275,0.363276561632091));
#8777=CARTESIAN_POINT('Ctrl Pts',(97.5785376134707,1.70133176282299,0.527521962657322));
#8778=CARTESIAN_POINT('Ctrl Pts',(97.5882996383161,1.65699991275731,0.653567004216802));
#8779=CARTESIAN_POINT('Ctrl Pts',(97.6033019644879,1.56752829277696,0.838538541028123));
#8780=CARTESIAN_POINT('Ctrl Pts',(97.6085459003841,1.53209652977743,0.901650740422808));
#8781=CARTESIAN_POINT('Ctrl Pts',(97.6148566838,1.48331286868377,0.977323332058229));
#8782=CARTESIAN_POINT('Ctrl Pts',(97.6160875494375,1.4734903662234,0.992070643697838));
#8783=CARTESIAN_POINT('Ctrl Pts',(97.6179052908165,1.45849829640912,1.01386541061438));
#8784=CARTESIAN_POINT('Ctrl Pts',(97.6185022169071,1.4534950569604,1.02102520976362));
#8785=CARTESIAN_POINT('Ctrl Pts',(97.6195272764258,1.44476095753207,1.03332967459584));
#8786=CARTESIAN_POINT('Ctrl Pts',(97.6199570313881,1.44105509690339,1.03849152716279));
#8787=CARTESIAN_POINT('Ctrl Pts',(97.6209654258572,1.43225530557543,1.0506108455963));
#8788=CARTESIAN_POINT('Ctrl Pts',(97.6215424769177,1.42713832285308,1.0575512396253));
#8789=CARTESIAN_POINT('Ctrl Pts',(97.6232220039917,1.41201362826333,1.077755841736));
#8790=CARTESIAN_POINT('Ctrl Pts',(97.6243156301994,1.40186979439358,1.09091762711231));
#8791=CARTESIAN_POINT('Ctrl Pts',(97.6328776694483,1.32025343362954,1.19379736865903));
#8792=CARTESIAN_POINT('Ctrl Pts',(97.6398601416418,1.24041753488387,1.27655507653146));
#8793=CARTESIAN_POINT('Ctrl Pts',(97.6538722981848,1.06682691655794,1.42471885462746));
#8794=CARTESIAN_POINT('Ctrl Pts',(97.6608748569019,0.973655896634358,1.48994404688947));
#8795=CARTESIAN_POINT('Ctrl Pts',(97.669688355139,0.855329321199499,1.55691421621624));
#8796=CARTESIAN_POINT('Ctrl Pts',(97.6711587363999,0.83554370618768,1.5676213716582));
#8797=CARTESIAN_POINT('Ctrl Pts',(97.6735495207309,0.803342261584215,1.58426463906003));
#8798=CARTESIAN_POINT('Ctrl Pts',(97.6744615391623,0.791051094788556,1.59043748171712));
#8799=CARTESIAN_POINT('Ctrl Pts',(97.6762218527198,0.76732268184386,1.60201120949056));
#8800=CARTESIAN_POINT('Ctrl Pts',(97.6770693205909,0.755896966967381,1.60743390981106));
#8801=CARTESIAN_POINT('Ctrl Pts',(97.679029059649,0.729477219176431,1.61962888119423));
#8802=CARTESIAN_POINT('Ctrl Pts',(97.6801441894382,0.714445254834644,1.62631567418661));
#8803=CARTESIAN_POINT('Ctrl Pts',(97.6838313674153,0.664762223535504,1.64759485489488));
#8804=CARTESIAN_POINT('Ctrl Pts',(97.686432936118,0.629742638082642,1.66129511508623));
#8805=CARTESIAN_POINT('Ctrl Pts',(97.6982401041299,0.47105139360017,1.71763922613347));
#8806=CARTESIAN_POINT('Ctrl Pts',(97.7078314111602,0.343343451211992,1.74764969268258));
#8807=CARTESIAN_POINT('Ctrl Pts',(97.7225976416918,0.142535472152848,1.77196529599101));
#8808=CARTESIAN_POINT('Ctrl Pts',(97.7277816840557,0.0710851755450795,1.77626749882615));
#8809=CARTESIAN_POINT('Ctrl Pts',(97.7340297739119,-0.0180668696401158,
1.77624561983836));
#8810=CARTESIAN_POINT('Ctrl Pts',(97.7352545122925,-0.0356975912649656,
1.77597878719614));
#8811=CARTESIAN_POINT('Ctrl Pts',(97.7370650612153,-0.0620359187743667,
1.77518776588008));
#8812=CARTESIAN_POINT('Ctrl Pts',(97.7376608108302,-0.0707477952616069,
1.77486191487761));
#8813=CARTESIAN_POINT('Ctrl Pts',(97.7387324464921,-0.0865075477073852,
1.77415622606674));
#8814=CARTESIAN_POINT('Ctrl Pts',(97.7392094808993,-0.0935558722339675,
1.77379851533988));
#8815=CARTESIAN_POINT('Ctrl Pts',(97.7402899875013,-0.10959472234161,1.77288865511995));
#8816=CARTESIAN_POINT('Ctrl Pts',(97.7408920047095,-0.118583389984603,1.77231012382063));
#8817=CARTESIAN_POINT('Ctrl Pts',(97.7427635291836,-0.146675619950463,1.7702873602638));
#8818=CARTESIAN_POINT('Ctrl Pts',(97.7440206133399,-0.165761174770733,1.76860238075398));
#8819=CARTESIAN_POINT('Ctrl Pts',(97.7469983195556,-0.211372283655386,1.7638307003064));
#8820=CARTESIAN_POINT('Ctrl Pts',(97.7487062545554,-0.237863310459977,1.76045396915936));
#8821=CARTESIAN_POINT('Ctrl Pts',(97.755466897655,-0.343509538651874,1.74455907919223));
#8822=CARTESIAN_POINT('Ctrl Pts',(97.7603695669039,-0.421857354911061,1.72728783200836));
#8823=CARTESIAN_POINT('Ctrl Pts',(97.7719887950462,-0.603533472988367,1.67413412309499));
#8824=CARTESIAN_POINT('Ctrl Pts',(97.7787054078985,-0.705231803194474,1.63389787011403));
#8825=CARTESIAN_POINT('Ctrl Pts',(97.7873151561424,-0.824466380498535,1.57350584355566));
#8826=CARTESIAN_POINT('Ctrl Pts',(97.788908784359,-0.846110762977519,1.56197373070925));
#8827=CARTESIAN_POINT('Ctrl Pts',(97.791539561245,-0.881093490031954,1.54239446335952));
#8828=CARTESIAN_POINT('Ctrl Pts',(97.7925673018254,-0.894577397893878,1.53461319954098));
#8829=CARTESIAN_POINT('Ctrl Pts',(97.7944331557519,-0.91871741597027,1.52025626636946));
#8830=CARTESIAN_POINT('Ctrl Pts',(97.7952689513567,-0.929409689604636,1.51374318195242));
#8831=CARTESIAN_POINT('Ctrl Pts',(97.7970765109963,-0.95226818095429,1.49948569408843));
#8832=CARTESIAN_POINT('Ctrl Pts',(97.7980495724369,-0.96441064730009,1.49170510396853));
#8833=CARTESIAN_POINT('Ctrl Pts',(97.8007719013291,-0.997921549224405,1.46965197228837));
#8834=CARTESIAN_POINT('Ctrl Pts',(97.8025329107228,-1.01907628718828,1.45506279536731));
#8835=CARTESIAN_POINT('Ctrl Pts',(97.8101401281606,-1.10820146556018,1.39070133401691));
#8836=CARTESIAN_POINT('Ctrl Pts',(97.8161488427617,-1.17289214131673,1.33659311260837));
#8837=CARTESIAN_POINT('Ctrl Pts',(97.8315215010746,-1.32533595371766,1.18947057894043));
#8838=CARTESIAN_POINT('Ctrl Pts',(97.8409922241215,-1.4073574069972,1.09119294837478));
#8839=CARTESIAN_POINT('Ctrl Pts',(97.8516596605576,-1.49103969379446,0.96561169987598));
#8840=CARTESIAN_POINT('Ctrl Pts',(97.853287338811,-1.50355984265597,0.945998546056781));
#8841=CARTESIAN_POINT('Ctrl Pts',(97.8555176095748,-1.52041168021235,0.918419474345613));
#8842=CARTESIAN_POINT('Ctrl Pts',(97.8561389019386,-1.52507263900095,0.910658806975379));
#8843=CARTESIAN_POINT('Ctrl Pts',(97.8572491516214,-1.53334470898269,0.896643860124756));
#8844=CARTESIAN_POINT('Ctrl Pts',(97.8577394416453,-1.53697739073637,0.89040255841188));
#8845=CARTESIAN_POINT('Ctrl Pts',(97.8587483952373,-1.54441268115744,0.877446903239372));
#8846=CARTESIAN_POINT('Ctrl Pts',(97.8592667165369,-1.5482097659704,0.870729650341733));
#8847=CARTESIAN_POINT('Ctrl Pts',(97.8606381682904,-1.55819196748425,0.852798830530928));
#8848=CARTESIAN_POINT('Ctrl Pts',(97.8614865912363,-1.56429992888596,0.841542517599367));
#8849=CARTESIAN_POINT('Ctrl Pts',(97.865799759499,-1.59496612214828,0.783540245267494));
#8850=CARTESIAN_POINT('Ctrl Pts',(97.8691583242864,-1.61755519354283,0.735777533661978));
#8851=CARTESIAN_POINT('Ctrl Pts',(97.8826352233069,-1.70087074363245,0.53715345997276));
#8852=CARTESIAN_POINT('Ctrl Pts',(97.8923040251559,-1.74287675597427,0.379313492927175));
#8853=CARTESIAN_POINT('Ctrl Pts',(97.9048635937319,-1.76699544275429,0.184242241589279));
#8854=CARTESIAN_POINT('Ctrl Pts',(97.9070593723809,-1.77019562383987,0.150417125199075));
#8855=CARTESIAN_POINT('Ctrl Pts',(97.9103378428348,-1.77347793073927,0.100490046205927));
#8856=CARTESIAN_POINT('Ctrl Pts',(97.9113971299915,-1.77431433485467,0.0844442606645976));
#8857=CARTESIAN_POINT('Ctrl Pts',(97.9132989634496,-1.77541785751231,0.0558043210656278));
#8858=CARTESIAN_POINT('Ctrl Pts',(97.914138826311,-1.77576890269678,0.0432143635474879));
#8859=CARTESIAN_POINT('Ctrl Pts',(97.9159175655818,-1.77622644058033,0.0166785196096828));
#8860=CARTESIAN_POINT('Ctrl Pts',(97.9168573342802,-1.7763026353616,0.00273303967374188));
#8861=CARTESIAN_POINT('Ctrl Pts',(97.9193884676931,-1.77606686676729,-0.0346191132123111));
#8862=CARTESIAN_POINT('Ctrl Pts',(97.9209890141123,-1.77545643032106,-0.0580204354177988));
#8863=CARTESIAN_POINT('Ctrl Pts',(97.9303005656727,-1.76927075674116,-0.192854587791792));
#8864=CARTESIAN_POINT('Ctrl Pts',(97.9383219233224,-1.75366936091735,-0.303558416506494));
#8865=CARTESIAN_POINT('Ctrl Pts',(97.9548536607572,-1.70113338126843,-0.523850692904557));
#8866=CARTESIAN_POINT('Ctrl Pts',(97.9633305628131,-1.66368074194744,-0.632806885667819));
#8867=CARTESIAN_POINT('Ctrl Pts',(97.9725374940179,-1.6090704094395,-0.752483809863521));
#8868=CARTESIAN_POINT('Ctrl Pts',(97.973689173362,-1.6019695329526,-0.767484939020849));
#8869=CARTESIAN_POINT('Ctrl Pts',(97.9754210735959,-1.59086308487221,-0.79012213038731));
#8870=CARTESIAN_POINT('Ctrl Pts',(97.9760098343347,-1.58701066898874,-0.797831736687428));
#8871=CARTESIAN_POINT('Ctrl Pts',(97.9770266913584,-1.58022042939027,-0.811176823038558));
#8872=CARTESIAN_POINT('Ctrl Pts',(97.9774563150506,-1.57730833768481,-0.816824861683276));
#8873=CARTESIAN_POINT('Ctrl Pts',(97.9784722324572,-1.57031946963772,-0.830203104135587));
#8874=CARTESIAN_POINT('Ctrl Pts',(97.9790568440424,-1.56621588280704,-0.837918998073964));
#8875=CARTESIAN_POINT('Ctrl Pts',(97.9808181821864,-1.55360975473148,-0.861205854619897));
#8876=CARTESIAN_POINT('Ctrl Pts',(97.9819844830017,-1.54493044487041,-0.876680542353074));
#8877=CARTESIAN_POINT('Ctrl Pts',(97.9878595995566,-1.49960128193414,-0.954735135648458));
#8878=CARTESIAN_POINT('Ctrl Pts',(97.9923840174514,-1.45937163277881,-1.01516497826087));
#8879=CARTESIAN_POINT('Ctrl Pts',(98.0051211547573,-1.33469436489176,-1.17964988082152));
#8880=CARTESIAN_POINT('Ctrl Pts',(98.0132080430048,-1.2420402602709,-1.2768386178051));
#8881=CARTESIAN_POINT('Ctrl Pts',(98.0239750277157,-1.11272924210098,-1.38495553804921));
#8882=CARTESIAN_POINT('Ctrl Pts',(98.0262177713969,-1.08546260600003,-1.4064277030494));
#8883=CARTESIAN_POINT('Ctrl Pts',(98.0295495057299,-1.04461920518179,-1.43669595192929));
#8884=CARTESIAN_POINT('Ctrl Pts',(98.0306138139149,-1.03152239950535,-1.44612795175987));
#8885=CARTESIAN_POINT('Ctrl Pts',(98.0325194317244,-1.0079986170815,-1.46258705585762));
#8886=CARTESIAN_POINT('Ctrl Pts',(98.0333579798927,-0.997622008173373,-1.46968446370513));
#8887=CARTESIAN_POINT('Ctrl Pts',(98.035142894318,-0.975487628671854,-1.48448154543761));
#8888=CARTESIAN_POINT('Ctrl Pts',(98.036090248123,-0.963712115236208,-1.4921529786152));
#8889=CARTESIAN_POINT('Ctrl Pts',(98.0386646325251,-0.93164735285255,-1.51250443763817));
#8890=CARTESIAN_POINT('Ctrl Pts',(98.0403014005506,-0.911191547132932,-1.5249151881083));
#8891=CARTESIAN_POINT('Ctrl Pts',(98.0496210260315,-0.794384693386821,-1.5925936399937));
#8892=CARTESIAN_POINT('Ctrl Pts',(98.0576098467225,-0.693282340216207,-1.6391318813214));
#8893=CARTESIAN_POINT('Ctrl Pts',(98.0740667416858,-0.480588425955996,-1.71382127789952));
#8894=CARTESIAN_POINT('Ctrl Pts',(98.0825016559088,-0.369245924892541,-1.74120931554221));
#8895=CARTESIAN_POINT('Ctrl Pts',(98.0916745135745,-0.239564446111824,-1.76009943371607));
#8896=CARTESIAN_POINT('Ctrl Pts',(98.0928297650041,-0.223058957020188,-1.76226725896373));
#8897=CARTESIAN_POINT('Ctrl Pts',(98.0945659201883,-0.197954466757662,-1.76520609197967));
#8898=CARTESIAN_POINT('Ctrl Pts',(98.0951554241278,-0.189376801999137,-1.76614692276035));
#8899=CARTESIAN_POINT('Ctrl Pts',(98.096172995095,-0.174471283318033,-1.76767197425584));
#8900=CARTESIAN_POINT('Ctrl Pts',(98.0966025983444,-0.168146831454844,-1.76828478573917));
#8901=CARTESIAN_POINT('Ctrl Pts',(98.0976177569636,-0.153127524129337,-1.76965877952667));
#8902=CARTESIAN_POINT('Ctrl Pts',(98.0982016389986,-0.144430183136867,-1.77038983413899));
#8903=CARTESIAN_POINT('Ctrl Pts',(98.0999584478457,-0.118096614105517,-1.77240794650525));
#8904=CARTESIAN_POINT('Ctrl Pts',(98.101121027297,-0.100445630535094,-1.7734958338457));
#8905=CARTESIAN_POINT('Ctrl Pts',(98.1069580150417,-0.0108759779991224,
-1.77767468756287));
#8906=CARTESIAN_POINT('Ctrl Pts',(98.1114506752503,0.0611742825880121,-1.77665572367131));
#8907=CARTESIAN_POINT('Ctrl Pts',(98.1240564817259,0.264826494166932,-1.76136733671736));
#8908=CARTESIAN_POINT('Ctrl Pts',(98.1320440159963,0.395155384570257,-1.73677815796907));
#8909=CARTESIAN_POINT('Ctrl Pts',(98.1427875808873,0.556178398088762,-1.68731802837179));
#8910=CARTESIAN_POINT('Ctrl Pts',(98.1451262653825,0.590474006407298,-1.67562427133545));
#8911=CARTESIAN_POINT('Ctrl Pts',(98.1485618274086,0.639577099906993,-1.65718692031408));
#8912=CARTESIAN_POINT('Ctrl Pts',(98.1496312881101,0.654688548133184,-1.65127533486647));
#8913=CARTESIAN_POINT('Ctrl Pts',(98.1515446157408,0.681400949134859,-1.64040115843671));
#8914=CARTESIAN_POINT('Ctrl Pts',(98.1523856776915,0.693034144509014,-1.63552036812227));
#8915=CARTESIAN_POINT('Ctrl Pts',(98.1541598759638,0.717339372620875,-1.62501706439367));
#8916=CARTESIAN_POINT('Ctrl Pts',(98.1550938299829,0.729999497315904,-1.61936930624657));
#8917=CARTESIAN_POINT('Ctrl Pts',(98.1575918864274,0.76349718098708,-1.60395315069062));
#8918=CARTESIAN_POINT('Ctrl Pts',(98.1591647545552,0.784212598631661,-1.59392727823774));
#8919=CARTESIAN_POINT('Ctrl Pts',(98.1687504837128,0.908153302718764,-1.53094133552961));
#8920=CARTESIAN_POINT('Ctrl Pts',(98.177102559885,1.0061635644245,-1.46838338638781));
#8921=CARTESIAN_POINT('Ctrl Pts',(98.193662273175,1.1844411984287,-1.32831724905043));
#8922=CARTESIAN_POINT('Ctrl Pts',(98.2018179603839,1.26493859002854,-1.25190326577961));
#8923=CARTESIAN_POINT('Ctrl Pts',(98.2107712597663,1.34904972000503,-1.15560433882296));
#8924=CARTESIAN_POINT('Ctrl Pts',(98.211958443334,1.36011387238599,-1.1425615270612));
#8925=CARTESIAN_POINT('Ctrl Pts',(98.2137248255919,1.37646531003053,-1.12271167898388));
#8926=CARTESIAN_POINT('Ctrl Pts',(98.2143132930364,1.38189391183424,-1.11602306789876));
#8927=CARTESIAN_POINT('Ctrl Pts',(98.2153298688578,1.39124246731377,-1.10433185387431));
#8928=CARTESIAN_POINT('Ctrl Pts',(98.2157595011614,1.39518443365512,-1.09934746350167));
#8929=CARTESIAN_POINT('Ctrl Pts',(98.2167757204004,1.40448652677752,-1.08745487489939));
#8930=CARTESIAN_POINT('Ctrl Pts',(98.2173606217157,1.40982250082346,-1.08052812692499));
#8931=CARTESIAN_POINT('Ctrl Pts',(98.2191237605207,1.42584362089369,-1.05941001590188));
#8932=CARTESIAN_POINT('Ctrl Pts',(98.2202915410238,1.43636759683231,-1.04509702842376));
#8933=CARTESIAN_POINT('Ctrl Pts',(98.2261818779144,1.48887793920055,-0.971389118555967));
#8934=CARTESIAN_POINT('Ctrl Pts',(98.2307189733209,1.527406738542,-0.909607234055698));
#8935=CARTESIAN_POINT('Ctrl Pts',(98.2435088905345,1.62608287019497,-0.727333496393834));
#8936=CARTESIAN_POINT('Ctrl Pts',(98.251635824275,1.67647483199959,-0.602154085750077));
#8937=CARTESIAN_POINT('Ctrl Pts',(98.2624129259529,1.72132495878054,-0.439621394110926));
#8938=CARTESIAN_POINT('Ctrl Pts',(98.2646176201938,1.72944580936269,-0.406501578108011));
#8939=CARTESIAN_POINT('Ctrl Pts',(98.2679035038079,1.73997654347827,-0.357495099775459));
#8940=CARTESIAN_POINT('Ctrl Pts',(98.2689610024306,1.74313240598006,-0.341775519017846));
#8941=CARTESIAN_POINT('Ctrl Pts',(98.2708590945617,1.74838028470816,-0.313668936708854));
#8942=CARTESIAN_POINT('Ctrl Pts',(98.2716970093455,1.7505545312382,-0.301298259295974));
#8943=CARTESIAN_POINT('Ctrl Pts',(98.2734855465802,1.75489320772866,-0.274978427330228));
#8944=CARTESIAN_POINT('Ctrl Pts',(98.2744372097997,1.75702290508012,-0.261024514166255));
#8945=CARTESIAN_POINT('Ctrl Pts',(98.2770362337843,1.76235455455678,-0.223062931168784));
#8946=CARTESIAN_POINT('Ctrl Pts',(98.2786936546126,1.76523204234351,-0.199013524262738));
#8947=CARTESIAN_POINT('Ctrl Pts',(98.2824231014625,1.77054965998076,-0.145275567998812));
#8948=CARTESIAN_POINT('Ctrl Pts',(98.2845023180137,1.77273645006418,-0.115569846465187));
#8949=CARTESIAN_POINT('Ctrl Pts',(98.2875024743817,1.77479247071467,-0.0730675819004155));
#8950=CARTESIAN_POINT('Ctrl Pts',(98.2884065155601,1.77527188706779,-0.060306055167887));
#8951=CARTESIAN_POINT('Ctrl Pts',(98.2893138640945,1.77561363880419,-0.0475422779488097));
#8952=CARTESIAN_POINT('Origin',(88.3562164250559,0.,0.));
#8953=CARTESIAN_POINT('',(99.1886897654568,1.7756136354609,-0.0475424028141329));
#8954=CARTESIAN_POINT('',(99.0404834457757,1.77561363837197,-0.0475422940912327));
#8955=CARTESIAN_POINT('',(88.3562164250559,1.77561363837197,-0.0475422940912398));
#8956=CARTESIAN_POINT('Ctrl Pts',(99.1886897654568,1.7756136354609,-0.0475424028141329));
#8957=CARTESIAN_POINT('Ctrl Pts',(99.1873699206532,1.77512914690477,-0.0656370811550229));
#8958=CARTESIAN_POINT('Ctrl Pts',(99.1860471354729,1.7743679485596,-0.0837286617151811));
#8959=CARTESIAN_POINT('Ctrl Pts',(99.1793003110797,1.76907863564114,-0.175857315182797));
#8960=CARTESIAN_POINT('Ctrl Pts',(99.1738633091114,1.76019369025663,-0.249567866918385));
#8961=CARTESIAN_POINT('Ctrl Pts',(99.1667114157917,1.74207524440372,-0.347698136066784));
#8962=CARTESIAN_POINT('Ctrl Pts',(99.164891219588,1.73687998037377,-0.372784416741384));
#8963=CARTESIAN_POINT('Ctrl Pts',(99.1617894940502,1.72698399410244,-0.415855038824187));
#8964=CARTESIAN_POINT('Ctrl Pts',(99.1604976011994,1.72254037392542,-0.433893832062961));
#8965=CARTESIAN_POINT('Ctrl Pts',(99.1586084370482,1.71555068728041,-0.460466159680731));
#8966=CARTESIAN_POINT('Ctrl Pts',(99.1579999776554,1.7132223131871,-0.469054963715754));
#8967=CARTESIAN_POINT('Ctrl Pts',(99.1569156947934,1.70893232588123,-0.484421452230894));
#8968=CARTESIAN_POINT('Ctrl Pts',(99.1564385712949,1.70699477678849,-0.491205328267051));
#8969=CARTESIAN_POINT('Ctrl Pts',(99.1553703744786,1.70254447867655,-0.506442617270516));
#8970=CARTESIAN_POINT('Ctrl Pts',(99.1547806007327,1.70000914543613,-0.514889056157521));
#8971=CARTESIAN_POINT('Ctrl Pts',(99.1529869324508,1.69206200152012,-0.540666132608314));
#8972=CARTESIAN_POINT('Ctrl Pts',(99.1517940331954,1.68644711371781,-0.557933579656584));
#8973=CARTESIAN_POINT('Ctrl Pts',(99.1451408457443,1.65332744171262,-0.654714378491946));
#8974=CARTESIAN_POINT('Ctrl Pts',(99.1399305756441,1.62046211518054,-0.732289831956704));
#8975=CARTESIAN_POINT('Ctrl Pts',(99.1300825417102,1.54769569438742,-0.874912545650337));
#8976=CARTESIAN_POINT('Ctrl Pts',(99.1254481941692,1.50887058439876,-0.940288872112908));
#8977=CARTESIAN_POINT('Ctrl Pts',(99.1163723231202,1.42648412994783,-1.06070714945549));
#8978=CARTESIAN_POINT('Ctrl Pts',(99.1119529097125,1.38361658356158,-1.11604664742778));
#8979=CARTESIAN_POINT('Ctrl Pts',(99.1060748640552,1.32413504167857,-1.18412387890668));
#8980=CARTESIAN_POINT('Ctrl Pts',(99.1047338502697,1.31040341616098,-1.19930221350897));
#8981=CARTESIAN_POINT('Ctrl Pts',(99.1025012126737,1.28730031616615,-1.22396881575017));
#8982=CARTESIAN_POINT('Ctrl Pts',(99.1016159952707,1.27807857362856,-1.23359511554692));
#8983=CARTESIAN_POINT('Ctrl Pts',(99.0998787946056,1.25986787591144,-1.25218131804407));
#8984=CARTESIAN_POINT('Ctrl Pts',(99.0990273049256,1.25088950074996,-1.26115049079156));
#8985=CARTESIAN_POINT('Ctrl Pts',(99.0969700306806,1.2290770269545,-1.28247852151722));
#8986=CARTESIAN_POINT('Ctrl Pts',(99.0957601899482,1.21615180271376,-1.29474176910311));
#8987=CARTESIAN_POINT('Ctrl Pts',(99.0922984825246,1.1789060009306,-1.32903017236865));
#8988=CARTESIAN_POINT('Ctrl Pts',(99.0900271611737,1.1541577104816,-1.35057776217391));
#8989=CARTESIAN_POINT('Ctrl Pts',(99.077599020635,1.01713832830286,-1.46335912793677));
#8990=CARTESIAN_POINT('Ctrl Pts',(99.0669424133231,0.894648189740849,-1.54129234742769));
#8991=CARTESIAN_POINT('Ctrl Pts',(99.0515812841342,0.704130242149068,-1.63207761749249));
#8992=CARTESIAN_POINT('Ctrl Pts',(99.0467963408315,0.642600006962748,-1.65727000778688));
#8993=CARTESIAN_POINT('Ctrl Pts',(99.0412330984514,0.567019447503088,-1.68337035249738));
#8994=CARTESIAN_POINT('Ctrl Pts',(99.0402995400953,0.554191478800444,-1.68763699598252));
#8995=CARTESIAN_POINT('Ctrl Pts',(99.0388351674416,0.533819995090226,-1.69415530905732));
#8996=CARTESIAN_POINT('Ctrl Pts',(99.038299083708,0.526308378360015,-1.69650390370777));
#8997=CARTESIAN_POINT('Ctrl Pts',(99.0372819774564,0.511948624279342,-1.70088909297112));
#8998=CARTESIAN_POINT('Ctrl Pts',(99.0368004945401,0.505103496033442,-1.70293439701532));
#8999=CARTESIAN_POINT('Ctrl Pts',(99.0356256872041,0.488289846014576,-1.70784796794033));
#9000=CARTESIAN_POINT('Ctrl Pts',(99.0349349586907,0.47830798897307,-1.71067037620324));
#9001=CARTESIAN_POINT('Ctrl Pts',(99.0325429061172,0.443428875501544,-1.72020340833021));
#9002=CARTESIAN_POINT('Ctrl Pts',(99.0308650970601,0.418409432791615,-1.72645956948996));
#9003=CARTESIAN_POINT('Ctrl Pts',(99.0221571154692,0.286229280981088,-1.75646894642826));
#9004=CARTESIAN_POINT('Ctrl Pts',(99.0154958048069,0.17716430432951,-1.77079875419169));
#9005=CARTESIAN_POINT('Ctrl Pts',(99.0026524058217,-0.0316621692219442,
-1.77873604865749));
#9006=CARTESIAN_POINT('Ctrl Pts',(98.9965074972078,-0.130919084806953,-1.77419315806105));
#9007=CARTESIAN_POINT('Ctrl Pts',(98.9884601664649,-0.254526036309295,-1.75810385154298));
#9008=CARTESIAN_POINT('Ctrl Pts',(98.9868007823962,-0.279705768338904,-1.75427399021902));
#9009=CARTESIAN_POINT('Ctrl Pts',(98.9841782154192,-0.318955226113086,-1.74743762863328));
#9010=CARTESIAN_POINT('Ctrl Pts',(98.9832266779609,-0.333086153989404,-1.74479921360548));
#9011=CARTESIAN_POINT('Ctrl Pts',(98.9814357495065,-0.359466984547717,-1.7395414440401));
#9012=CARTESIAN_POINT('Ctrl Pts',(98.9805977288283,-0.371724289320995,-1.73696343869477));
#9013=CARTESIAN_POINT('Ctrl Pts',(98.9787041946085,-0.399218392198995,-1.7308764227673));
#9014=CARTESIAN_POINT('Ctrl Pts',(98.9776464288059,-0.414438015027777,-1.72729546399883));
#9015=CARTESIAN_POINT('Ctrl Pts',(98.974411174572,-0.460554014717092,-1.715800460705));
#9016=CARTESIAN_POINT('Ctrl Pts',(98.9722136802158,-0.491284830873417,-1.70725516785119));
#9017=CARTESIAN_POINT('Ctrl Pts',(98.9604427056008,-0.652703533446317,-1.65765059066628));
#9018=CARTESIAN_POINT('Ctrl Pts',(98.9504144440548,-0.778527243201682,-1.60240774180693));
#9019=CARTESIAN_POINT('Ctrl Pts',(98.9345701423892,-0.965804983480632,-1.49287910030096));
#9020=CARTESIAN_POINT('Ctrl Pts',(98.9287660000946,-1.03207821052265,-1.44785518781079));
#9021=CARTESIAN_POINT('Ctrl Pts',(98.9222204793852,-1.10608561051922,-1.38990415039842));
#9022=CARTESIAN_POINT('Ctrl Pts',(98.9212557619064,-1.1169749239136,-1.38116833693476));
#9023=CARTESIAN_POINT('Ctrl Pts',(98.9197539215046,-1.13391468846448,-1.36724723206105));
#9024=CARTESIAN_POINT('Ctrl Pts',(98.9192110885588,-1.14003490586894,-1.36214827899283));
#9025=CARTESIAN_POINT('Ctrl Pts',(98.9181841629665,-1.15161196418613,-1.35237036688754));
#9026=CARTESIAN_POINT('Ctrl Pts',(98.9176995756184,-1.15707495317854,-1.34769925418989));
#9027=CARTESIAN_POINT('Ctrl Pts',(98.9165326220393,-1.17022669439044,-1.33631497922606));
#9028=CARTESIAN_POINT('Ctrl Pts',(98.9158526686074,-1.17788635874265,-1.32956834284475));
#9029=CARTESIAN_POINT('Ctrl Pts',(98.9135447430441,-1.20385341605598,-1.30629600114507));
#9030=CARTESIAN_POINT('Ctrl Pts',(98.9119381097314,-1.22187547872979,-1.28945443899491));
#9031=CARTESIAN_POINT('Ctrl Pts',(98.9032271258343,-1.3188448833139,-1.1949774074261));
#9032=CARTESIAN_POINT('Ctrl Pts',(98.8965070480947,-1.3907585348469,-1.11045884628892));
#9033=CARTESIAN_POINT('Ctrl Pts',(98.883214932035,-1.51493909851543,-0.933362196504009));
#9034=CARTESIAN_POINT('Ctrl Pts',(98.8766740599553,-1.56770794998903,-0.841720424503123));
#9035=CARTESIAN_POINT('Ctrl Pts',(98.8683838946422,-1.62140276711668,-0.725682798524403));
#9036=CARTESIAN_POINT('Ctrl Pts',(98.8669244105442,-1.63039497666059,-0.705247902836286));
#9037=CARTESIAN_POINT('Ctrl Pts',(98.864546954758,-1.64428707962536,-0.671991263311253));
#9038=CARTESIAN_POINT('Ctrl Pts',(98.8636371929861,-1.64942785463916,-0.659272320560589));
#9039=CARTESIAN_POINT('Ctrl Pts',(98.8618782609334,-1.65902827709649,-0.634704261344452));
#9040=CARTESIAN_POINT('Ctrl Pts',(98.8610298838408,-1.6635095913183,-0.622864470650001));
#9041=CARTESIAN_POINT('Ctrl Pts',(98.8590636856041,-1.67355051486739,-0.59545449483932));
#9042=CARTESIAN_POINT('Ctrl Pts',(98.8579429444778,-1.679019982512,-0.579852780675154));
#9043=CARTESIAN_POINT('Ctrl Pts',(98.8543210889802,-1.69587996198853,-0.529519733712121));
#9044=CARTESIAN_POINT('Ctrl Pts',(98.851792545761,-1.7064158976022,-0.494514345614418));
#9045=CARTESIAN_POINT('Ctrl Pts',(98.8400231928364,-1.74983619067927,-0.332272339746914));
#9046=CARTESIAN_POINT('Ctrl Pts',(98.830389147513,-1.76961272206897,-0.201971393440725));
#9047=CARTESIAN_POINT('Ctrl Pts',(98.8155637833109,-1.7776965858352,0.000943296622551324));
#9048=CARTESIAN_POINT('Ctrl Pts',(98.8103646717862,-1.77620987103552,0.0727083615184915));
#9049=CARTESIAN_POINT('Ctrl Pts',(98.8041007872244,-1.76895462034831,0.161787635620858));
#9050=CARTESIAN_POINT('Ctrl Pts',(98.8028744860854,-1.76725930524357,0.179360795521043));
#9051=CARTESIAN_POINT('Ctrl Pts',(98.8010620916201,-1.76433531814633,0.205574856701156));
#9052=CARTESIAN_POINT('Ctrl Pts',(98.8004660308916,-1.76330457451399,0.214236136412348));
#9053=CARTESIAN_POINT('Ctrl Pts',(98.7994418672879,-1.76141272178564,0.229193498241413));
#9054=CARTESIAN_POINT('Ctrl Pts',(98.7990121526483,-1.7605815881873,0.235492910486742));
#9055=CARTESIAN_POINT('Ctrl Pts',(98.7980030010624,-1.75854126144492,0.250342266186049));
#9056=CARTESIAN_POINT('Ctrl Pts',(98.7974251625246,-1.75730350907491,0.258888012897894));
#9057=CARTESIAN_POINT('Ctrl Pts',(98.7957056589216,-1.75341307735095,0.284433946764175));
#9058=CARTESIAN_POINT('Ctrl Pts',(98.7945737065931,-1.75057557837745,0.30140552127845));
#9059=CARTESIAN_POINT('Ctrl Pts',(98.7846299695859,-1.72322291174428,0.451557777221006));
#9060=CARTESIAN_POINT('Ctrl Pts',(98.7764901417329,-1.68379547072324,0.581588340186751));
#9061=CARTESIAN_POINT('Ctrl Pts',(98.7628513182545,-1.59583225269337,0.784704088004222));
#9062=CARTESIAN_POINT('Ctrl Pts',(98.7574997962186,-1.55603159358649,0.860932253593579));
#9063=CARTESIAN_POINT('Ctrl Pts',(98.7502865302608,-1.49724771444616,0.9560257364921));
#9064=CARTESIAN_POINT('Ctrl Pts',(98.7485984007624,-1.48313805091659,0.977771618172882));
#9065=CARTESIAN_POINT('Ctrl Pts',(98.7459406468328,-1.46041969772443,1.01116154987498));
#9066=CARTESIAN_POINT('Ctrl Pts',(98.7449832047023,-1.45213557271491,1.02302279107987));
#9067=CARTESIAN_POINT('Ctrl Pts',(98.7431870959099,-1.43641631867426,1.04495400442521));
#9068=CARTESIAN_POINT('Ctrl Pts',(98.7423498765059,-1.42901780303677,1.05504920106986));
#9069=CARTESIAN_POINT('Ctrl Pts',(98.7404660198791,-1.41221560484216,1.07747463633437));
#9070=CARTESIAN_POINT('Ctrl Pts',(98.7394172292792,-1.40275599756727,1.08976148360643));
#9071=CARTESIAN_POINT('Ctrl Pts',(98.7363080390735,-1.37441226648112,1.12559585276744));
#9072=CARTESIAN_POINT('Ctrl Pts',(98.7342302778677,-1.35508823527885,1.14878665677154));
#9073=CARTESIAN_POINT('Ctrl Pts',(98.7204325224175,-1.22434633752994,1.29779948090917));
#9074=CARTESIAN_POINT('Ctrl Pts',(98.7079785404145,-1.09615172853382,1.40774210732993));
#9075=CARTESIAN_POINT('Ctrl Pts',(98.6919632391324,-0.909565392296823,1.52662703229225));
#9076=CARTESIAN_POINT('Ctrl Pts',(98.688156376503,-0.863390584741517,1.55320865574977));
#9077=CARTESIAN_POINT('Ctrl Pts',(98.683564517283,-0.804687215404461,1.58357420751393));
#9078=CARTESIAN_POINT('Ctrl Pts',(98.6826791809479,-0.793223580484867,1.58934740090699));
#9079=CARTESIAN_POINT('Ctrl Pts',(98.6812728054071,-0.774763722303712,1.59839446637652));
#9080=CARTESIAN_POINT('Ctrl Pts',(98.6807471543394,-0.767807223784897,1.60174772308159));
#9081=CARTESIAN_POINT('Ctrl Pts',(98.6797356776823,-0.754306483941104,1.60814734767734));
#9082=CARTESIAN_POINT('Ctrl Pts',(98.679249538319,-0.747765220445794,1.61119934860822));
#9083=CARTESIAN_POINT('Ctrl Pts',(98.6781599952481,-0.732991115181813,1.6179832475312));
#9084=CARTESIAN_POINT('Ctrl Pts',(98.6775579467952,-0.724747900945792,1.62169240391921));
#9085=CARTESIAN_POINT('Ctrl Pts',(98.6754247116542,-0.695271945151755,1.6346858998415));
#9086=CARTESIAN_POINT('Ctrl Pts',(98.673912859204,-0.673885264126018,1.64361791247423));
#9087=CARTESIAN_POINT('Ctrl Pts',(98.6623046201056,-0.506408404264219,1.70974467585286));
#9088=CARTESIAN_POINT('Ctrl Pts',(98.6530023601573,-0.353483373276005,1.74778090353368));
#9089=CARTESIAN_POINT('Ctrl Pts',(98.6391131644428,-0.132089153537259,1.77255557785057));
#9090=CARTESIAN_POINT('Ctrl Pts',(98.6349425856815,-0.0662934287961824,
1.7762332539265));
#9091=CARTESIAN_POINT('Ctrl Pts',(98.6293500445639,0.0196696588200166,1.77625504264761));
#9092=CARTESIAN_POINT('Ctrl Pts',(98.6280311999854,0.0397874647733673,1.77591829080341));
#9093=CARTESIAN_POINT('Ctrl Pts',(98.6258254644194,0.0731474008574148,1.7747927648004));
#9094=CARTESIAN_POINT('Ctrl Pts',(98.6249446590548,0.0863945041916861,1.77419724767929));
#9095=CARTESIAN_POINT('Ctrl Pts',(98.623198839252,0.112496560855711,1.77273082261834));
#9096=CARTESIAN_POINT('Ctrl Pts',(98.622334139683,0.125351176102582,1.77186825501714));
#9097=CARTESIAN_POINT('Ctrl Pts',(98.6202384786548,0.156320656236037,1.76945145617547));
#9098=CARTESIAN_POINT('Ctrl Pts',(98.6190032497908,0.174422929146081,1.76775880768756));
#9099=CARTESIAN_POINT('Ctrl Pts',(98.6144680747016,0.240312758147703,1.76057590224795));
#9100=CARTESIAN_POINT('Ctrl Pts',(98.6111171043335,0.287894255387175,1.75342347104452));
#9101=CARTESIAN_POINT('Ctrl Pts',(98.6021363238702,0.412514997033795,1.7294814229272));
#9102=CARTESIAN_POINT('Ctrl Pts',(98.5964240258592,0.488824131830416,1.70948043519826));
#9103=CARTESIAN_POINT('Ctrl Pts',(98.5826450819672,0.667703891289564,1.64963590685902));
#9104=CARTESIAN_POINT('Ctrl Pts',(98.5745590136591,0.768412630883759,1.60520181897494));
#9105=CARTESIAN_POINT('Ctrl Pts',(98.565665923048,0.87935361551117,1.54340375703528));
#9106=CARTESIAN_POINT('Ctrl Pts',(98.5644758319805,0.8942088587139,1.53484478359516));
#9107=CARTESIAN_POINT('Ctrl Pts',(98.5627060092614,0.916346437940334,1.5216594930648));
#9108=CARTESIAN_POINT('Ctrl Pts',(98.5621169579187,0.923722319863408,1.517193293806));
#9109=CARTESIAN_POINT('Ctrl Pts',(98.5610998026773,0.936477317073108,1.50934246592391));
#9110=CARTESIAN_POINT('Ctrl Pts',(98.5606701681046,0.941871065149031,1.50598251801909));
#9111=CARTESIAN_POINT('Ctrl Pts',(98.5596544760855,0.954636450601399,1.49793511712676));
#9112=CARTESIAN_POINT('Ctrl Pts',(98.5590700977939,0.961991682806987,1.49322214629639));
#9113=CARTESIAN_POINT('Ctrl Pts',(98.5573102784046,0.984161856493525,1.47878448003472));
#9114=CARTESIAN_POINT('Ctrl Pts',(98.5561452363389,0.998866819080417,1.4688918389474));
#9115=CARTESIAN_POINT('Ctrl Pts',(98.5502832049804,1.07282868776984,1.4175101612288));
#9116=CARTESIAN_POINT('Ctrl Pts',(98.5457696994683,1.1296657879425,1.37264487609026));
#9117=CARTESIAN_POINT('Ctrl Pts',(98.5330777487624,1.28300535612447,1.23560909922294));
#9118=CARTESIAN_POINT('Ctrl Pts',(98.5250250721187,1.37207628615552,1.135886130672));
#9119=CARTESIAN_POINT('Ctrl Pts',(98.5142664367791,1.46952153370502,0.998404293647805));
#9120=CARTESIAN_POINT('Ctrl Pts',(98.5119909188176,1.48902885531175,0.96907041697685));
#9121=CARTESIAN_POINT('Ctrl Pts',(98.5086310911144,1.51614024153341,0.925548837737813));
#9122=CARTESIAN_POINT('Ctrl Pts',(98.5075724747417,1.52444470690188,0.911806004866494));
#9123=CARTESIAN_POINT('Ctrl Pts',(98.5056713691768,1.53892810815905,0.887086774543881));
#9124=CARTESIAN_POINT('Ctrl Pts',(98.5048315551604,1.54517882786778,0.876153550208527));
#9125=CARTESIAN_POINT('Ctrl Pts',(98.5030524136949,1.55810824428382,0.852969766428469));
#9126=CARTESIAN_POINT('Ctrl Pts',(98.5021121885454,1.56475988554641,0.840705182908352));
#9127=CARTESIAN_POINT('Ctrl Pts',(98.4995785587272,1.58219644296248,0.807630979510274));
#9128=CARTESIAN_POINT('Ctrl Pts',(98.4979759411601,1.59271478525861,0.786684755368459));
#9129=CARTESIAN_POINT('Ctrl Pts',(98.4886126614864,1.65120819412982,0.664216375875407));
#9130=CARTESIAN_POINT('Ctrl Pts',(98.4805373497161,1.68987658660363,0.55855251845839));
#9131=CARTESIAN_POINT('Ctrl Pts',(98.4640172343482,1.74719880700822,0.339652453129529));
#9132=CARTESIAN_POINT('Ctrl Pts',(98.4556095231236,1.76539796340563,0.226806767744066));
#9133=CARTESIAN_POINT('Ctrl Pts',(98.4464588489229,1.7737135582986,0.0963452210403971));
#9134=CARTESIAN_POINT('Ctrl Pts',(98.4453013659596,1.77454000222293,0.0796870077196417));
#9135=CARTESIAN_POINT('Ctrl Pts',(98.4435625411103,1.77543811335797,0.054388791647298));
#9136=CARTESIAN_POINT('Ctrl Pts',(98.4429725613684,1.77568155931224,0.0457563415994727));
#9137=CARTESIAN_POINT('Ctrl Pts',(98.4419545159736,1.77599483952051,0.0307695705511481));
#9138=CARTESIAN_POINT('Ctrl Pts',(98.4415249086054,1.77609354557589,0.0244163263853195));
#9139=CARTESIAN_POINT('Ctrl Pts',(98.4405101703523,1.77624684551325,0.00934160670781613));
#9140=CARTESIAN_POINT('Ctrl Pts',(98.4399267076147,1.77627130396795,0.000620094314811771));
#9141=CARTESIAN_POINT('Ctrl Pts',(98.4384718880171,1.77617155357579,-0.0212499771479));
#9142=CARTESIAN_POINT('Ctrl Pts',(98.4376047832566,1.77596558586547,-0.0343977292065965));
#9143=CARTESIAN_POINT('Ctrl Pts',(98.436744300164,1.7756136383717,-0.047542294101169));
#9144=CARTESIAN_POINT('',(98.4812164250559,0.00162964136512414,1.77624925243307));
#9145=CARTESIAN_POINT('Ctrl Pts',(98.2893138640945,1.77561363880419,-0.0475422779488097));
#9146=CARTESIAN_POINT('Ctrl Pts',(98.2931977998273,1.77707651853614,0.00709349711413117));
#9147=CARTESIAN_POINT('Ctrl Pts',(98.2971436447791,1.77601699051399,0.0617704143106846));
#9148=CARTESIAN_POINT('Ctrl Pts',(98.3086015490245,1.76570929891744,0.218842284437513));
#9149=CARTESIAN_POINT('Ctrl Pts',(98.3161848227136,1.75009763405617,0.320593896543771));
#9150=CARTESIAN_POINT('Ctrl Pts',(98.3259897503879,1.71763954577045,0.45382854040931));
#9151=CARTESIAN_POINT('Ctrl Pts',(98.3284180199761,1.70853369093817,0.486989676364695));
#9152=CARTESIAN_POINT('Ctrl Pts',(98.3316004842894,1.69508870632277,0.530916033474651));
#9153=CARTESIAN_POINT('Ctrl Pts',(98.3323956139171,1.69159928941403,0.541931193820995));
#9154=CARTESIAN_POINT('Ctrl Pts',(98.3336429375755,1.68591446006054,0.559286592704036));
#9155=CARTESIAN_POINT('Ctrl Pts',(98.3340990689852,1.68379026039922,0.565649557764315));
#9156=CARTESIAN_POINT('Ctrl Pts',(98.3350506856983,1.679262107583,0.578961920465669));
#9157=CARTESIAN_POINT('Ctrl Pts',(98.3355457022361,1.67685096121182,0.585908685881759));
#9158=CARTESIAN_POINT('Ctrl Pts',(98.3367823785789,1.6706890459633,0.603312174024025));
#9159=CARTESIAN_POINT('Ctrl Pts',(98.3375208724404,1.66688310862648,0.613749285611066));
#9160=CARTESIAN_POINT('Ctrl Pts',(98.3404610780624,1.6512336725457,0.655445473337094));
#9161=CARTESIAN_POINT('Ctrl Pts',(98.3426214107926,1.6386059998908,0.686405218803319));
#9162=CARTESIAN_POINT('Ctrl Pts',(98.3485818342248,1.60082477898677,0.77203888233926));
#9163=CARTESIAN_POINT('Ctrl Pts',(98.3523084282866,1.57375555523373,0.825819871699164));
#9164=CARTESIAN_POINT('Ctrl Pts',(98.3646400300355,1.47470643534915,0.999977647631338));
#9165=CARTESIAN_POINT('Ctrl Pts',(98.3731414198256,1.39123372698692,1.11318418275383));
#9166=CARTESIAN_POINT('Ctrl Pts',(98.3837976143028,1.27834344994996,1.23349830291792));
#9167=CARTESIAN_POINT('Ctrl Pts',(98.3854151378637,1.26098438101382,1.25123871886078));
#9168=CARTESIAN_POINT('Ctrl Pts',(98.3879953173562,1.2329895117206,1.27867420360461));
#9169=CARTESIAN_POINT('Ctrl Pts',(98.388947190896,1.22259743628979,1.28861411729099));
#9170=CARTESIAN_POINT('Ctrl Pts',(98.3907383379673,1.20293128586108,1.30697254318422));
#9171=CARTESIAN_POINT('Ctrl Pts',(98.3915762360143,1.19368658332831,1.31542131427491));
#9172=CARTESIAN_POINT('Ctrl Pts',(98.3934689356629,1.17270905378348,1.33418951707691));
#9173=CARTESIAN_POINT('Ctrl Pts',(98.3945259822322,1.16092797662998,1.34445319670272));
#9174=CARTESIAN_POINT('Ctrl Pts',(98.3976834925259,1.12555424127244,1.37445917576315));
#9175=CARTESIAN_POINT('Ctrl Pts',(98.3998021300482,1.10158350881587,1.39374457630302));
#9176=CARTESIAN_POINT('Ctrl Pts',(98.4048402368584,1.04406461931032,1.43760976514977));
#9177=CARTESIAN_POINT('Ctrl Pts',(98.4077779307064,1.01013114047404,1.46165228186317));
#9178=CARTESIAN_POINT('Ctrl Pts',(98.4186470344951,0.883069555781208,1.54513891247854));
#9179=CARTESIAN_POINT('Ctrl Pts',(98.4267824020307,0.785299093422799,1.59704971862112));
#9180=CARTESIAN_POINT('Ctrl Pts',(98.4396543716882,0.622084332889818,1.66507691792306));
#9181=CARTESIAN_POINT('Ctrl Pts',(98.4444369679918,0.559425251202567,1.68716191560871));
#9182=CARTESIAN_POINT('Ctrl Pts',(98.4500171997923,0.482445674826527,1.7095320726339));
#9183=CARTESIAN_POINT('Ctrl Pts',(98.45096870659,0.469175784994432,1.71322148266652));
#9184=CARTESIAN_POINT('Ctrl Pts',(98.4524546603536,0.448204245114866,1.71879022078136));
#9185=CARTESIAN_POINT('Ctrl Pts',(98.4529946289523,0.440530952882375,1.72077289440693));
#9186=CARTESIAN_POINT('Ctrl Pts',(98.4540196554321,0.425858955921624,1.72445936167206));
#9187=CARTESIAN_POINT('Ctrl Pts',(98.4545051697931,0.418862844188094,1.72617202500167));
#9188=CARTESIAN_POINT('Ctrl Pts',(98.4556791516275,0.401837539283828,1.73023025492238));
#9189=CARTESIAN_POINT('Ctrl Pts',(98.4563651303312,0.391797807747294,1.73253127926466));
#9190=CARTESIAN_POINT('Ctrl Pts',(98.4578326756743,0.370137305477898,1.73729776906998));
#9191=CARTESIAN_POINT('Ctrl Pts',(98.458612741806,0.358510606196195,1.73973426879071));
#9192=CARTESIAN_POINT('Ctrl Pts',(98.4669475181434,0.233184267069116,1.76468796792731));
#9193=CARTESIAN_POINT('Ctrl Pts',(98.4739989313469,0.11755406777982,1.77614329398991));
#9194=CARTESIAN_POINT('Ctrl Pts',(98.4811171398043,0.00162354587747538,
1.77624925801498));
#9195=CARTESIAN_POINT('Ctrl Pts',(98.4812164250559,0.00162964136512414,
1.77624925243307));
#9196=CARTESIAN_POINT('Ctrl Pts',(98.4854530653849,-0.0614205339738133,
1.77630709857919));
#9197=CARTESIAN_POINT('Ctrl Pts',(98.4896897057139,-0.124559988590764,1.7730036213554));
#9198=CARTESIAN_POINT('Ctrl Pts',(98.4939263460429,-0.187397282201051,1.76633697836049));
#9199=CARTESIAN_POINT('Ctrl Pts',(98.4981600988292,-0.250191748156839,1.75967487911128));
#9200=CARTESIAN_POINT('Ctrl Pts',(98.5023938516155,-0.312683948257245,1.74965421013642));
#9201=CARTESIAN_POINT('Ctrl Pts',(98.5066276044018,-0.374485080126635,1.73632513869452));
#9202=CARTESIAN_POINT('Ctrl Pts',(98.5108600832926,-0.436267616631049,1.72300007784176));
#9203=CARTESIAN_POINT('Ctrl Pts',(98.5150925621835,-0.497358992103221,1.70636869804803));
#9204=CARTESIAN_POINT('Ctrl Pts',(98.5193250410744,-0.557380291560129,1.68653232197914));
#9205=CARTESIAN_POINT('Ctrl Pts',(98.5236537296518,-0.618765952317672,1.66624503958037));
#9206=CARTESIAN_POINT('Ctrl Pts',(98.5279824182292,-0.679031739625796,1.64260538592702));
#9207=CARTESIAN_POINT('Ctrl Pts',(98.5323111068066,-0.737790779831893,1.61577499290435));
#9208=CARTESIAN_POINT('Ctrl Pts',(98.5365485336318,-0.795311003045761,1.58951026512515));
#9209=CARTESIAN_POINT('Ctrl Pts',(98.540785960457,-0.85138696102605,1.56018834574077));
#9210=CARTESIAN_POINT('Ctrl Pts',(98.5450233872823,-0.905680318337323,1.52800759928621));
#9211=CARTESIAN_POINT('Ctrl Pts',(98.5493977067357,-0.961727655288556,1.49478723441652));
#9212=CARTESIAN_POINT('Ctrl Pts',(98.5537720261892,-1.01587472029036,1.45852045930447));
#9213=CARTESIAN_POINT('Ctrl Pts',(98.5581463456427,-1.06778385824547,1.41947232962478));
#9214=CARTESIAN_POINT('Ctrl Pts',(98.5625206650961,-1.1196929962006,1.38042419994509));
#9215=CARTESIAN_POINT('Ctrl Pts',(98.5668949845496,-1.16936380077856,1.33859516044597));
#9216=CARTESIAN_POINT('Ctrl Pts',(98.571269304003,-1.21650027826686,1.29429175052484));
#9217=CARTESIAN_POINT('Ctrl Pts',(98.5755681123442,-1.26282306853283,1.25075312237103));
#9218=CARTESIAN_POINT('Ctrl Pts',(98.5798669206853,-1.3068998404826,1.20463586732403));
#9219=CARTESIAN_POINT('Ctrl Pts',(98.5841657290265,-1.34843003259545,1.15620089504144));
#9220=CARTESIAN_POINT('Ctrl Pts',(98.5885929911513,-1.39120119892496,1.10631862505256));
#9221=CARTESIAN_POINT('Ctrl Pts',(98.5930202532761,-1.43127069973378,1.05397820182919));
#9222=CARTESIAN_POINT('Ctrl Pts',(98.5974475154009,-1.46834877583047,0.999507846400997));
#9223=CARTESIAN_POINT('Ctrl Pts',(98.6017345078096,-1.5042521007911,0.946763284720955));
#9224=CARTESIAN_POINT('Ctrl Pts',(98.6060215002182,-1.53735042392031,0.892022197397326));
#9225=CARTESIAN_POINT('Ctrl Pts',(98.6103084926268,-1.56742121352955,0.83561642030153));
#9226=CARTESIAN_POINT('Ctrl Pts',(98.6145928647598,-1.59747362341002,0.779245119283622));
#9227=CARTESIAN_POINT('Ctrl Pts',(98.6188772368928,-1.62450193288729,0.721211590003397));
#9228=CARTESIAN_POINT('Ctrl Pts',(98.6231616090258,-1.64832841992064,0.661874219608161));
#9229=CARTESIAN_POINT('Ctrl Pts',(98.6274449047247,-1.67214892062964,0.602551757526726));
#9230=CARTESIAN_POINT('Ctrl Pts',(98.6317282004237,-1.69276900815509,0.54192657205303));
#9231=CARTESIAN_POINT('Ctrl Pts',(98.6360114961226,-1.71005899179161,0.480377254970144));
#9232=CARTESIAN_POINT('Ctrl Pts',(98.6402952574559,-1.72735085501084,0.418821246901651));
#9233=CARTESIAN_POINT('Ctrl Pts',(98.644579018789,-1.7413117627366,0.356341393772886));
#9234=CARTESIAN_POINT('Ctrl Pts',(98.6488627801223,-1.75186235659193,0.293329756513333));
#9235=CARTESIAN_POINT('Ctrl Pts',(98.6531512994025,-1.76242466892624,0.230248132620194));
#9236=CARTESIAN_POINT('Ctrl Pts',(98.6574398186828,-1.7695690292107,0.166634044264517));
#9237=CARTESIAN_POINT('Ctrl Pts',(98.6617283379631,-1.77326770929479,0.102886800282689));
#9238=CARTESIAN_POINT('Ctrl Pts',(98.6660197376141,-1.77696887358597,0.0390967406608165));
#9239=CARTESIAN_POINT('Ctrl Pts',(98.6703111372652,-1.7772197523833,-0.0248261489702147));
#9240=CARTESIAN_POINT('Ctrl Pts',(98.6746025369162,-1.77404474419002,-0.0884833776015348));
#9241=CARTESIAN_POINT('Ctrl Pts',(98.6789011723523,-1.77086438257393,-0.152247939517972));
#9242=CARTESIAN_POINT('Ctrl Pts',(98.6831998077884,-1.7642466664396,-0.215745447224884));
#9243=CARTESIAN_POINT('Ctrl Pts',(98.6874984432244,-1.75426757065288,-0.27858455279439));
#9244=CARTESIAN_POINT('Ctrl Pts',(98.688472302157,-1.75200679936507,-0.292820797105429));
#9245=CARTESIAN_POINT('Ctrl Pts',(98.6894461610895,-1.74957370910265,-0.307023303107869));
#9246=CARTESIAN_POINT('Ctrl Pts',(98.6904200200221,-1.74696953940082,-0.321187625704485));
#9247=CARTESIAN_POINT('Ctrl Pts',(98.6947188303473,-1.73547420755271,-0.383711810874786));
#9248=CARTESIAN_POINT('Ctrl Pts',(98.6990176406726,-1.72059461319993,-0.44574538270941));
#9249=CARTESIAN_POINT('Ctrl Pts',(98.7033164509978,-1.7023871991581,-0.506894354518425));
#9250=CARTESIAN_POINT('Ctrl Pts',(98.7077437128746,-1.68363573445878,-0.569870501688007));
#9251=CARTESIAN_POINT('Ctrl Pts',(98.7121709747514,-1.66135438932414,-0.631907792220913));
#9252=CARTESIAN_POINT('Ctrl Pts',(98.7165982366282,-1.63566203412561,-0.692584848679265));
#9253=CARTESIAN_POINT('Ctrl Pts',(98.7208852309857,-1.61078368158352,-0.751339493402278));
#9254=CARTESIAN_POINT('Ctrl Pts',(98.7251722253433,-1.58270745083389,-0.808818307680883));
#9255=CARTESIAN_POINT('Ctrl Pts',(98.7294592197008,-1.55159167589601,-0.864654459185978));
#9256=CARTESIAN_POINT('Ctrl Pts',(98.7337435937645,-1.52049491952074,-0.92045648255688));
#9257=CARTESIAN_POINT('Ctrl Pts',(98.7380279678283,-1.48636254800156,-0.974617394987629));
#9258=CARTESIAN_POINT('Ctrl Pts',(98.7423123418921,-1.44939949033832,-1.02679364037134));
#9259=CARTESIAN_POINT('Ctrl Pts',(98.7465956395009,-1.41244571969531,-1.0789567764));
#9260=CARTESIAN_POINT('Ctrl Pts',(98.7508789371096,-1.37266296594167,-1.12913582427183));
#9261=CARTESIAN_POINT('Ctrl Pts',(98.7551622347184,-1.33029916432395,-1.17701665064646));
#9262=CARTESIAN_POINT('Ctrl Pts',(98.7594459979375,-1.28793075760369,-1.22490268184469));
#9263=CARTESIAN_POINT('Ctrl Pts',(98.7637297611566,-1.24298108247334,-1.27048962054459));
#9264=CARTESIAN_POINT('Ctrl Pts',(98.7680135243757,-1.19573666601708,-1.31349833956589));
#9265=CARTESIAN_POINT('Ctrl Pts',(98.772302045495,-1.14843977602159,-1.35655482761206));
#9266=CARTESIAN_POINT('Ctrl Pts',(98.7765905666143,-1.0988434344109,-1.39702704480607));
#9267=CARTESIAN_POINT('Ctrl Pts',(98.7808790877336,-1.04726823442091,-1.43467533179912));
#9268=CARTESIAN_POINT('Ctrl Pts',(98.7851704891983,-0.99565839442585,-1.4723489049152));
#9269=CARTESIAN_POINT('Ctrl Pts',(98.7894618906631,-0.942067474509896,-1.50719450071351));
#9270=CARTESIAN_POINT('Ctrl Pts',(98.7937532921278,-0.886843623844741,-1.53901671509634));
#9271=CARTESIAN_POINT('Ctrl Pts',(98.798051929325,-0.831526660240488,-1.57089258491742));
#9272=CARTESIAN_POINT('Ctrl Pts',(98.8023505665221,-0.774571723567137,-1.59973468013227));
#9273=CARTESIAN_POINT('Ctrl Pts',(98.8066492037192,-0.716348904436194,-1.62539481653322));
#9274=CARTESIAN_POINT('Ctrl Pts',(98.8076230478266,-0.703158689322715,-1.6312080479092));
#9275=CARTESIAN_POINT('Ctrl Pts',(98.8085968919339,-0.689903467078543,-1.63685817102858));
#9276=CARTESIAN_POINT('Ctrl Pts',(98.8095707360413,-0.676587645183508,-1.64234381932805));
#9277=CARTESIAN_POINT('Ctrl Pts',(98.813869548981,-0.617807983189047,-1.66655896394362));
#9278=CARTESIAN_POINT('Ctrl Pts',(98.8181683619208,-0.557607015386957,-1.68766382635497));
#9279=CARTESIAN_POINT('Ctrl Pts',(98.8224671748606,-0.49634646777098,-1.7054923765386));
#9280=CARTESIAN_POINT('Ctrl Pts',(98.8268944364106,-0.433255453858138,-1.72385364413176));
#9281=CARTESIAN_POINT('Ctrl Pts',(98.8313216979606,-0.369040983373696,-1.73873937573369));
#9282=CARTESIAN_POINT('Ctrl Pts',(98.8357489595106,-0.304121627727075,-1.75002117074298));
#9283=CARTESIAN_POINT('Ctrl Pts',(98.8400359565544,-0.241259047189839,-1.76094553590823));
#9284=CARTESIAN_POINT('Ctrl Pts',(98.8443229535983,-0.177736118936162,-1.76849082743003));
#9285=CARTESIAN_POINT('Ctrl Pts',(98.8486099506421,-0.113946952508602,-1.77259136704261));
#9286=CARTESIAN_POINT('Ctrl Pts',(98.8528943274113,-0.0501967749438444,
-1.77668940034597));
#9287=CARTESIAN_POINT('Ctrl Pts',(98.8571787041804,0.0138188162689568,-1.77734682486678));
#9288=CARTESIAN_POINT('Ctrl Pts',(98.8614630809496,0.0777000290380064,-1.77454973669027));
#9289=CARTESIAN_POINT('Ctrl Pts',(98.8657463812783,0.141565191790422,-1.77175335127611));
#9290=CARTESIAN_POINT('Ctrl Pts',(98.870029681607,0.205295539914834,-1.76550419818667));
#9291=CARTESIAN_POINT('Ctrl Pts',(98.8743129819358,0.268492709345181,-1.75584046186676));
#9292=CARTESIAN_POINT('Ctrl Pts',(98.878596747885,0.331696748688168,-1.74617567504056));
#9293=CARTESIAN_POINT('Ctrl Pts',(98.8828805138343,0.39436699676,-1.73309564767349));
#9294=CARTESIAN_POINT('Ctrl Pts',(98.8871642797835,0.456113602137702,-1.71668996747956));
#9295=CARTESIAN_POINT('Ctrl Pts',(98.8914528036302,0.517928788296557,-1.70026606580841));
#9296=CARTESIAN_POINT('Ctrl Pts',(98.8957413274769,0.578817797915282,-1.68050927369018));
#9297=CARTESIAN_POINT('Ctrl Pts',(98.9000298513236,0.638405494324399,-1.65755919572015));
#9298=CARTESIAN_POINT('Ctrl Pts',(98.9043212555173,0.698033212253346,-1.63459370354457));
#9299=CARTESIAN_POINT('Ctrl Pts',(98.908612659711,0.756357419068994,-1.60843086550882));
#9300=CARTESIAN_POINT('Ctrl Pts',(98.9129040639047,0.813025244011015,-1.5792574252163));
#9301=CARTESIAN_POINT('Ctrl Pts',(98.9172027038082,0.869788616219608,-1.55003479576787));
#9302=CARTESIAN_POINT('Ctrl Pts',(98.9215013437118,0.924889603182745,-1.51779169480434));
#9303=CARTESIAN_POINT('Ctrl Pts',(98.9257999836153,0.978003133856311,-1.48275889229073));
#9304=CARTESIAN_POINT('Ctrl Pts',(98.9267738064304,0.990035583448879,-1.47482248842178));
#9305=CARTESIAN_POINT('Ctrl Pts',(98.9277476292454,1.00196616811946,-1.46674307731022));
#9306=CARTESIAN_POINT('Ctrl Pts',(98.9287214520604,1.01379135144946,-1.45852362278651));
#9307=CARTESIAN_POINT('Ctrl Pts',(98.9330204332438,1.06599411343148,-1.42223850008274));
#9308=CARTESIAN_POINT('Ctrl Pts',(98.9373194144271,1.11635265359479,-1.38307333437165));
#9309=CARTESIAN_POINT('Ctrl Pts',(98.9416183956104,1.16453139310864,-1.34124222158581));
#9310=CARTESIAN_POINT('Ctrl Pts',(98.9459097161208,1.2126242793583,-1.29948565075798));
#9311=CARTESIAN_POINT('Ctrl Pts',(98.9502010366311,1.25854470208939,-1.2550728955287));
#9312=CARTESIAN_POINT('Ctrl Pts',(98.9544923571415,1.30198733371713,-1.20826033839573));
#9313=CARTESIAN_POINT('Ctrl Pts',(98.9587793843407,1.34538650256142,-1.16149461553492));
#9314=CARTESIAN_POINT('Ctrl Pts',(98.96306641154,1.38631245406923,-1.11233421824034));
#9315=CARTESIAN_POINT('Ctrl Pts',(98.9673534387392,1.42449525816556,-1.06107366472071));
#9316=CARTESIAN_POINT('Ctrl Pts',(98.9716377202399,1.46265360744384,-1.00984594188335));
#9317=CARTESIAN_POINT('Ctrl Pts',(98.9759220017406,1.49807199391404,-0.956521134085841));
#9318=CARTESIAN_POINT('Ctrl Pts',(98.9802062832412,1.53052079063424,-0.901426742412457));
#9319=CARTESIAN_POINT('Ctrl Pts',(98.9844893630292,1.56296048568047,-0.846347804353431));
#9320=CARTESIAN_POINT('Ctrl Pts',(98.988772442817,1.59243198974081,-0.789500702131185));
#9321=CARTESIAN_POINT('Ctrl Pts',(98.9930555226049,1.61875011542024,-0.731240129045819));
#9322=CARTESIAN_POINT('Ctrl Pts',(98.9973414405387,1.64508568057823,-0.672940950095153));
#9323=CARTESIAN_POINT('Ctrl Pts',(99.0016273584724,1.66826348222424,-0.613226887845016));
#9324=CARTESIAN_POINT('Ctrl Pts',(99.0059132764061,1.68814583070561,-0.552474177470106));
#9325=CARTESIAN_POINT('Ctrl Pts',(99.0102006152251,1.70803477066555,-0.49170132610487));
#9326=CARTESIAN_POINT('Ctrl Pts',(99.0144879540441,1.72462594499934,-0.429889626563904));
#9327=CARTESIAN_POINT('Ctrl Pts',(99.0187752928631,1.7378318986038,-0.367429387359163));
#9328=CARTESIAN_POINT('Ctrl Pts',(99.0230691702742,1.75105799252098,-0.304873890455651));
#9329=CARTESIAN_POINT('Ctrl Pts',(99.0273630476853,1.76088847299791,-0.241668376698973));
#9330=CARTESIAN_POINT('Ctrl Pts',(99.0316569250965,1.76728741874363,-0.178211228744057));
#9331=CARTESIAN_POINT('Ctrl Pts',(99.0345990986562,1.77167198941965,-0.13473026154056));
#9332=CARTESIAN_POINT('Ctrl Pts',(99.037541272216,1.77444653737116,-0.0911312814132852));
#9333=CARTESIAN_POINT('Ctrl Pts',(99.0404834457757,1.77561363837197,-0.0475422940912327));
#9334=CARTESIAN_POINT('Origin',(88.3562164250559,0.,0.));
#9335=CARTESIAN_POINT('',(99.9383713772532,1.77277786422444,-0.0474589613121508));
#9336=CARTESIAN_POINT('',(99.7906304259994,1.77562736014833,-0.0475451276261121));
#9337=CARTESIAN_POINT('',(88.3562164250559,1.77561363837197,-0.0475422940912398));
#9338=CARTESIAN_POINT('',(99.3790868291567,-0.00134908208039473,1.77778173587435));
#9339=CARTESIAN_POINT('Ctrl Pts',(99.3790868291567,-0.00134908208039473,
1.77778173587435));
#9340=CARTESIAN_POINT('Ctrl Pts',(99.3849459429476,-0.0883230632624573,
1.77851575880056));
#9341=CARTESIAN_POINT('Ctrl Pts',(99.4305219620782,-0.764095661216901,1.73316171652182));
#9342=CARTESIAN_POINT('Ctrl Pts',(99.5158148865485,-1.91281695310219,0.866461694035085));
#9343=CARTESIAN_POINT('Ctrl Pts',(99.6349656025676,-1.76465526215908,-1.13813616919857));
#9344=CARTESIAN_POINT('Ctrl Pts',(99.7541163185868,0.000461911234235865,
-2.10006451370548));
#9345=CARTESIAN_POINT('Ctrl Pts',(99.8552515768152,1.49850875722623,-1.28264712973566));
#9346=CARTESIAN_POINT('Ctrl Pts',(99.9166699297041,1.76334219989321,-0.371393921105317));
#9347=CARTESIAN_POINT('Ctrl Pts',(99.9383713772532,1.77277786422444,-0.0474589613121508));
#9348=CARTESIAN_POINT('Ctrl Pts',(99.3782063185287,-0.00140217910956735,
1.77624944655692));
#9349=CARTESIAN_POINT('Ctrl Pts',(99.3685348291268,0.154290094078351,1.77637235072075));
#9350=CARTESIAN_POINT('Ctrl Pts',(99.3592174787437,0.309321614980016,1.75602653963719));
#9351=CARTESIAN_POINT('Ctrl Pts',(99.3472577925782,0.489394120042289,1.70777661516411));
#9352=CARTESIAN_POINT('Ctrl Pts',(99.3452660430548,0.518851342200709,1.69905876162217));
#9353=CARTESIAN_POINT('Ctrl Pts',(99.3422376731009,0.562731298362937,1.68482498703638));
#9354=CARTESIAN_POINT('Ctrl Pts',(99.3412195560868,0.577333250838938,1.67987738943743));
#9355=CARTESIAN_POINT('Ctrl Pts',(99.3393636079286,0.603667558597018,1.67057060461596));
#9356=CARTESIAN_POINT('Ctrl Pts',(99.3385279745531,0.615421877887082,1.66627625702889));
#9357=CARTESIAN_POINT('Ctrl Pts',(99.3367120993374,0.640737028222907,1.65672316751608));
#9358=CARTESIAN_POINT('Ctrl Pts',(99.3357304632278,0.654280522423058,1.65142137843329));
#9359=CARTESIAN_POINT('Ctrl Pts',(99.3330079721719,0.691443889802688,1.63634434706927));
#9360=CARTESIAN_POINT('Ctrl Pts',(99.3312556571195,0.714919401590681,1.62622495542015));
#9361=CARTESIAN_POINT('Ctrl Pts',(99.3186330643329,0.880800968754984,1.5504338359959));
#9362=CARTESIAN_POINT('Ctrl Pts',(99.3071143631717,1.01415424533639,1.46667224023185));
#9363=CARTESIAN_POINT('Ctrl Pts',(99.292198655096,1.17162133479598,1.33591326794866));
#9364=CARTESIAN_POINT('Ctrl Pts',(99.288728587195,1.20723939567059,1.30381533076926));
#9365=CARTESIAN_POINT('Ctrl Pts',(99.2839139085717,1.25567423697466,1.25647845770651));
#9366=CARTESIAN_POINT('Ctrl Pts',(99.2825177311901,1.26959932237344,1.24240634859454));
#9367=CARTESIAN_POINT('Ctrl Pts',(99.2801075291702,1.29347094434881,1.21746208974287));
#9368=CARTESIAN_POINT('Ctrl Pts',(99.2790872479893,1.30352268678777,1.20669369104589));
#9369=CARTESIAN_POINT('Ctrl Pts',(99.2775470268664,1.31863112074085,1.19009894334054));
#9370=CARTESIAN_POINT('Ctrl Pts',(99.2770203539084,1.32378547008393,1.18436293522051));
#9371=CARTESIAN_POINT('Ctrl Pts',(99.2760645086134,1.33312098478529,1.17383683860203));
#9372=CARTESIAN_POINT('Ctrl Pts',(99.2756344966678,1.33731394811641,1.16905769383451));
#9373=CARTESIAN_POINT('Ctrl Pts',(99.2746272215611,1.34711931762362,1.15775973024393));
#9374=CARTESIAN_POINT('Ctrl Pts',(99.2740515276798,1.35271014090362,1.15122253769098));
#9375=CARTESIAN_POINT('Ctrl Pts',(99.272345371931,1.36923069168006,1.13161899441757));
#9376=CARTESIAN_POINT('Ctrl Pts',(99.2712243977414,1.38002053471065,1.11843534091929));
#9377=CARTESIAN_POINT('Ctrl Pts',(99.261236343838,1.47536863006348,0.998452377114076));
#9378=CARTESIAN_POINT('Ctrl Pts',(99.2530512342777,1.54758089085957,0.882396668867394));
#9379=CARTESIAN_POINT('Ctrl Pts',(99.2393878065869,1.64234494390321,0.681959696256119));
#9380=CARTESIAN_POINT('Ctrl Pts',(99.2340621501052,1.67324281528213,0.602181059079847));
#9381=CARTESIAN_POINT('Ctrl Pts',(99.2268803999771,1.70585656694848,0.495768337278834));
#9382=CARTESIAN_POINT('Ctrl Pts',(99.2251960080795,1.71289347520407,0.470880773358365));
#9383=CARTESIAN_POINT('Ctrl Pts',(99.2225428039142,1.72301280476698,0.43185635354207));
#9384=CARTESIAN_POINT('Ctrl Pts',(99.2215861024424,1.72647027081705,0.417819839986028));
#9385=CARTESIAN_POINT('Ctrl Pts',(99.2197906095763,1.73260120769771,0.391553072020312));
#9386=CARTESIAN_POINT('Ctrl Pts',(99.2189532553555,1.73531746886852,0.379333654603007));
#9387=CARTESIAN_POINT('Ctrl Pts',(99.217068072029,1.7411124427657,0.351898427725253));
#9388=CARTESIAN_POINT('Ctrl Pts',(99.2160180766663,1.74412125401575,0.336669075429469));
#9389=CARTESIAN_POINT('Ctrl Pts',(99.2133033188218,1.75133931929291,0.297436497642581));
#9390=CARTESIAN_POINT('Ctrl Pts',(99.2116294618974,1.7552547924634,0.273383233761641));
#9391=CARTESIAN_POINT('Ctrl Pts',(99.2030565709261,1.77261059972131,0.150926969981673));
#9392=CARTESIAN_POINT('Ctrl Pts',(99.195924614015,1.77826940326188,0.0516452116294196));
#9393=CARTESIAN_POINT('Ctrl Pts',(99.1886897654568,1.7756136354609,-0.0475424028141329));
#9394=CARTESIAN_POINT('',(99.2312164566968,-0.000376088333153419,1.7759924949984));
#9395=CARTESIAN_POINT('Ctrl Pts',(99.0404834457757,1.77561363837197,-0.0475422940912327));
#9396=CARTESIAN_POINT('Ctrl Pts',(99.0429463532103,1.77659062415254,-0.0110537461648616));
#9397=CARTESIAN_POINT('Ctrl Pts',(99.0454092606449,1.77644140601071,0.025427782505673));
#9398=CARTESIAN_POINT('Ctrl Pts',(99.0478721680795,1.77517361646096,0.0618279380290967));
#9399=CARTESIAN_POINT('Ctrl Pts',(99.0521709862975,1.77296078591098,0.125361650056849));
#9400=CARTESIAN_POINT('Ctrl Pts',(99.0564698045155,1.7673283209483,0.188905764324683));
#9401=CARTESIAN_POINT('Ctrl Pts',(99.0607686227335,1.75827434492677,0.252062274988406));
#9402=CARTESIAN_POINT('Ctrl Pts',(99.0651958836237,1.74894984877258,0.317105813804496));
#9403=CARTESIAN_POINT('Ctrl Pts',(99.0696231445139,1.73599602715012,0.381737676937767));
#9404=CARTESIAN_POINT('Ctrl Pts',(99.0740504054041,1.71946874504975,0.445523621480441));
#9405=CARTESIAN_POINT('Ctrl Pts',(99.0783374074591,1.70346505923033,0.507288781048526));
#9406=CARTESIAN_POINT('Ctrl Pts',(99.0826244095141,1.68411109550379,0.568260292570386));
#9407=CARTESIAN_POINT('Ctrl Pts',(99.0869114115691,1.66150974684009,0.628052086737548));
#9408=CARTESIAN_POINT('Ctrl Pts',(99.0911957932383,1.63892221301767,0.687807333787172));
#9409=CARTESIAN_POINT('Ctrl Pts',(99.0954801749075,1.61309140837735,0.746383823106717));
#9410=CARTESIAN_POINT('Ctrl Pts',(99.0997645565767,1.58416972777763,0.803411685310175));
#9411=CARTESIAN_POINT('Ctrl Pts',(99.1040478616877,1.55525531447471,0.860425217834618));
#9412=CARTESIAN_POINT('Ctrl Pts',(99.1083311667986,1.52325179482111,0.915890446506549));
#9413=CARTESIAN_POINT('Ctrl Pts',(99.1126144719096,1.48835841589744,0.969460307762655));
#9414=CARTESIAN_POINT('Ctrl Pts',(99.1168982425165,1.45346124487328,1.02303599081944));
#9415=CARTESIAN_POINT('Ctrl Pts',(99.1211820131233,1.41567386897964,1.07471547726131));
#9416=CARTESIAN_POINT('Ctrl Pts',(99.1254657837301,1.37523883859957,1.12418067912027));
#9417=CARTESIAN_POINT('Ctrl Pts',(99.129754312023,1.33475889984356,1.17370081853858));
#9418=CARTESIAN_POINT('Ctrl Pts',(99.1340428403159,1.2916257609992,1.22100137764623));
#9419=CARTESIAN_POINT('Ctrl Pts',(99.1383313686088,1.24612145243364,1.2657983205411));
#9420=CARTESIAN_POINT('Ctrl Pts',(99.1426227771303,1.2005865826129,1.31062534961564));
#9421=CARTESIAN_POINT('Ctrl Pts',(99.1469141856517,1.15267775279318,1.35294508455562));
#9422=CARTESIAN_POINT('Ctrl Pts',(99.1512055941731,1.10271073464048,1.39251323089177));
#9423=CARTESIAN_POINT('Ctrl Pts',(99.1555042381955,1.05265946992754,1.43214809083917));
#9424=CARTESIAN_POINT('Ctrl Pts',(99.1598028822179,1.00054350676621,1.46902181997348));
#9425=CARTESIAN_POINT('Ctrl Pts',(99.1641015262402,0.946707238453464,1.50293362034383));
#9426=CARTESIAN_POINT('Ctrl Pts',(99.1650753121931,0.934511531722722,1.51061577189315));
#9427=CARTESIAN_POINT('Ctrl Pts',(99.1660490981459,0.92222763750181,1.51814611481939));
#9428=CARTESIAN_POINT('Ctrl Pts',(99.1670228840987,0.909859714797821,1.52552265204029));
#9429=CARTESIAN_POINT('Ctrl Pts',(99.1714716133702,0.853357010482439,1.55922227253753));
#9430=CARTESIAN_POINT('Ctrl Pts',(99.1759203426416,0.794882235523169,1.58983725820357));
#9431=CARTESIAN_POINT('Ctrl Pts',(99.180369071913,0.734792781678399,1.61714057227358));
#9432=CARTESIAN_POINT('Ctrl Pts',(99.1848065217802,0.674855679932851,1.64437466093134));
#9433=CARTESIAN_POINT('Ctrl Pts',(99.1892439716474,0.613312456593282,1.66831359787621));
#9434=CARTESIAN_POINT('Ctrl Pts',(99.1936814215145,0.550545679536776,1.68877574510158));
#9435=CARTESIAN_POINT('Ctrl Pts',(99.1981122123532,0.487873093010735,1.70920718594705));
#9436=CARTESIAN_POINT('Ctrl Pts',(99.2025430031918,0.423981029782271,1.72617206002377));
#9437=CARTESIAN_POINT('Ctrl Pts',(99.2069737940304,0.359272284467834,1.73953657280129));
#9438=CARTESIAN_POINT('Ctrl Pts',(99.2113975132016,0.294666816141035,1.75287975543844));
#9439=CARTESIAN_POINT('Ctrl Pts',(99.2158212323728,0.229247702670285,1.7626339160979));
#9440=CARTESIAN_POINT('Ctrl Pts',(99.2202449515439,0.16343141159382,1.76871541979043));
#9441=CARTESIAN_POINT('Ctrl Pts',(99.2239021093813,0.109020054221916,1.77374309402368));
#9442=CARTESIAN_POINT('Ctrl Pts',(99.2275592672186,0.0543376437225603,1.77626153193324));
#9443=CARTESIAN_POINT('Ctrl Pts',(99.2312164250559,-0.000375670171088504,
1.77624996027359));
#9444=CARTESIAN_POINT('Ctrl Pts',(99.2312167715186,-0.000380248985858326,
1.77343075235475));
#9445=CARTESIAN_POINT('Ctrl Pts',(99.249535714385,-0.274007951532822,1.77394632845611));
#9446=CARTESIAN_POINT('Ctrl Pts',(99.307571562591,-1.14020838492317,1.58562537855393));
#9447=CARTESIAN_POINT('Ctrl Pts',(99.4053243161369,-2.08671183082761,0.235097532724869));
#9448=CARTESIAN_POINT('Ctrl Pts',(99.524475032156,-1.32822316119735,-1.62647487068021));
#9449=CARTESIAN_POINT('Ctrl Pts',(99.6436257481753,0.647387598188645,-1.99764857090965));
#9450=CARTESIAN_POINT('Ctrl Pts',(99.7323442127897,1.67669836196288,-0.910947872649348));
#9451=CARTESIAN_POINT('Ctrl Pts',(99.7813457720644,1.77332763342921,-0.185653457768005));
#9452=CARTESIAN_POINT('Ctrl Pts',(99.7906304259995,1.77562736014833,-0.0475451276259355));
#9453=CARTESIAN_POINT('Origin',(66.9212607628943,0.,0.));
#9454=CARTESIAN_POINT('',(33.4926516271063,2.69912154532077E-16,2.204));
#9455=CARTESIAN_POINT('Origin',(33.4926516271063,0.,0.));
#9456=CARTESIAN_POINT('',(90.3498698986825,-0.214101726762253,-2.19357617843498));
#9457=CARTESIAN_POINT('',(90.3498698986825,1.62325119196235,-1.49086269246796));
#9458=CARTESIAN_POINT('Origin',(90.3498698986825,0.,0.));
#9459=CARTESIAN_POINT('',(90.6260484068025,0.00185087634597349,2.20399922283488));
#9460=CARTESIAN_POINT('Ctrl Pts',(90.3498698986825,1.62325119196235,-1.49086269246796));
#9461=CARTESIAN_POINT('Ctrl Pts',(90.3895868040222,2.11930827345322,-0.950755777941539));
#9462=CARTESIAN_POINT('Ctrl Pts',(90.4690206147016,2.5208914807363,0.654645457688011));
#9463=CARTESIAN_POINT('Ctrl Pts',(90.5610799237519,1.20144938824896,2.06273780995529));
#9464=CARTESIAN_POINT('Ctrl Pts',(90.6134223274625,0.235399057971462,2.20457276789839));
#9465=CARTESIAN_POINT('Ctrl Pts',(90.6260478258334,0.00186055395922385,
2.2027266091469));
#9466=CARTESIAN_POINT('',(91.3760484068552,-0.00126552574240722,2.2039996366707));
#9467=CARTESIAN_POINT('Ctrl Pts',(90.6260484068025,0.00185087634597349,
2.20399922283488));
#9468=CARTESIAN_POINT('Ctrl Pts',(90.6300874787337,-0.0729039514327416,
2.20406200050787));
#9469=CARTESIAN_POINT('Ctrl Pts',(90.634126550665,-0.147719807169649,2.20031720231216));
#9470=CARTESIAN_POINT('Ctrl Pts',(90.6381656225962,-0.222177953843929,2.19277289221336));
#9471=CARTESIAN_POINT('Ctrl Pts',(90.6422034326244,-0.29661283800512,2.1852309391382));
#9472=CARTESIAN_POINT('Ctrl Pts',(90.6462412426525,-0.370689755210188,2.17389187899442));
#9473=CARTESIAN_POINT('Ctrl Pts',(90.6502790526807,-0.443993956851574,2.15881573235867));
#9474=CARTESIAN_POINT('Ctrl Pts',(90.6543169380162,-0.517299525655997,2.14373930454462));
#9475=CARTESIAN_POINT('Ctrl Pts',(90.6583548233517,-0.589831878086408,2.12492575105078));
#9476=CARTESIAN_POINT('Ctrl Pts',(90.6623927086872,-0.661186999955675,2.10248608820359));
#9477=CARTESIAN_POINT('Ctrl Pts',(90.6664347773491,-0.732616047094706,2.08002317743688));
#9478=CARTESIAN_POINT('Ctrl Pts',(90.670476846011,-0.802864967400653,2.05392680203279));
#9479=CARTESIAN_POINT('Ctrl Pts',(90.6745189146728,-0.871546247179227,2.02435746325292));
#9480=CARTESIAN_POINT('Ctrl Pts',(90.6785631757033,-0.940264778844592,1.99477208642507));
#9481=CARTESIAN_POINT('Ctrl Pts',(90.6826074367339,-1.00741354460176,1.9617102103385));
#9482=CARTESIAN_POINT('Ctrl Pts',(90.6866516977644,-1.07262878263828,1.92537879251225));
#9483=CARTESIAN_POINT('Ctrl Pts',(90.6907031775646,-1.13796042606586,1.88898252522707));
#9484=CARTESIAN_POINT('Ctrl Pts',(90.6947546573649,-1.20135124130891,1.84930531944377));
#9485=CARTESIAN_POINT('Ctrl Pts',(90.6988061371651,-1.26246612799149,1.80659770720384));
#9486=CARTESIAN_POINT('Ctrl Pts',(90.7016447736901,-1.30528577861491,1.77667496441006));
#9487=CARTESIAN_POINT('Ctrl Pts',(90.704483410215,-1.34698881701027,1.7452654959714));
#9488=CARTESIAN_POINT('Ctrl Pts',(90.70732204674,-1.38747039308724,1.71246661523848));
#9489=CARTESIAN_POINT('Ctrl Pts',(90.7114017643054,-1.44565092995657,1.6653277270162));
#9490=CARTESIAN_POINT('Ctrl Pts',(90.7154814818708,-1.50153452025124,1.61513293526345));
#9491=CARTESIAN_POINT('Ctrl Pts',(90.7195611994362,-1.5547836346165,1.56213438907435));
#9492=CARTESIAN_POINT('Ctrl Pts',(90.7236350692713,-1.60795642348694,1.50921180922406));
#9493=CARTESIAN_POINT('Ctrl Pts',(90.7277089391064,-1.65850190012224,1.45349378779541));
#9494=CARTESIAN_POINT('Ctrl Pts',(90.7317828089415,-1.70611547319863,1.3952727303693));
#9495=CARTESIAN_POINT('Ctrl Pts',(90.7358520916738,-1.75367543426419,1.33711722878705));
#9496=CARTESIAN_POINT('Ctrl Pts',(90.7399213744061,-1.79830975135764,1.27646465745508));
#9497=CARTESIAN_POINT('Ctrl Pts',(90.7439906571384,-1.83975172184307,1.21364311145224));
#9498=CARTESIAN_POINT('Ctrl Pts',(90.7480574630342,-1.88116846798516,1.1508598028263));
#9499=CARTESIAN_POINT('Ctrl Pts',(90.75212426893,-1.91939646253376,1.08591053571015));
#9500=CARTESIAN_POINT('Ctrl Pts',(90.7561910748258,-1.95421105246868,1.01915414065256));
#9501=CARTESIAN_POINT('Ctrl Pts',(90.7602567070635,-1.98901559510216,0.952417011127753));
#9502=CARTESIAN_POINT('Ctrl Pts',(90.7643223393013,-2.0204084694443,0.883874210752672));
#9503=CARTESIAN_POINT('Ctrl Pts',(90.768387971539,-2.0482107022416,0.813909650528229));
#9504=CARTESIAN_POINT('Ctrl Pts',(90.772453731708,-2.07601380987793,0.74394288876377));
#9505=CARTESIAN_POINT('Ctrl Pts',(90.7765194918769,-2.10022587761992,0.672554720968091));
#9506=CARTESIAN_POINT('Ctrl Pts',(90.7805852520459,-2.12071646269066,0.600148052461083));
#9507=CARTESIAN_POINT('Ctrl Pts',(90.7846552374533,-2.14122834208392,0.527666137154293));
#9508=CARTESIAN_POINT('Ctrl Pts',(90.7887252228607,-2.15801088618608,0.454164066194615));
#9509=CARTESIAN_POINT('Ctrl Pts',(90.7927952082681,-2.17098405606415,0.380058190696185));
#9510=CARTESIAN_POINT('Ctrl Pts',(90.7968673685232,-2.18396415831782,0.305912715796166));
#9511=CARTESIAN_POINT('Ctrl Pts',(90.8009395287782,-2.19313077453104,0.231163266298682));
#9512=CARTESIAN_POINT('Ctrl Pts',(90.8050116890333,-2.19845572220061,0.156231999037993));
#9513=CARTESIAN_POINT('Ctrl Pts',(90.8090911138956,-2.20379016941132,0.0811670567253429));
#9514=CARTESIAN_POINT('Ctrl Pts',(90.813170538758,-2.20526924949307,0.00592012497610547));
#9515=CARTESIAN_POINT('Ctrl Pts',(90.8172499636204,-2.20291694593774,-0.0690863901239109));
#9516=CARTESIAN_POINT('Ctrl Pts',(90.8203242299999,-2.20114424317238,-0.125611516924139));
#9517=CARTESIAN_POINT('Ctrl Pts',(90.8233984963795,-2.19719672128774,-0.182000103923053));
#9518=CARTESIAN_POINT('Ctrl Pts',(90.826472762759,-2.19110394319517,-0.23807458939287));
#9519=CARTESIAN_POINT('Ctrl Pts',(90.8305414997454,-2.18304025953379,-0.312288175614706));
#9520=CARTESIAN_POINT('Ctrl Pts',(90.8346102367318,-2.17118595693924,-0.386237671673184));
#9521=CARTESIAN_POINT('Ctrl Pts',(90.8386789737183,-2.15556753379367,-0.459504741275533));
#9522=CARTESIAN_POINT('Ctrl Pts',(90.8427416649012,-2.13997231832122,-0.53266294212804));
#9523=CARTESIAN_POINT('Ctrl Pts',(90.8468043560841,-2.12062418510459,-0.60514026552376));
#9524=CARTESIAN_POINT('Ctrl Pts',(90.850867047267,-2.09760134521141,-0.676523906870472));
#9525=CARTESIAN_POINT('Ctrl Pts',(90.8549249084732,-2.07460587628337,-0.747822682963042));
#9526=CARTESIAN_POINT('Ctrl Pts',(90.8589827696795,-2.04794452602362,-0.818029906979268));
#9527=CARTESIAN_POINT('Ctrl Pts',(90.8630406308857,-2.01774609217716,-0.8867450070363));
#9528=CARTESIAN_POINT('Ctrl Pts',(90.8670958721175,-1.98756715607173,-0.955415740910866));
#9529=CARTESIAN_POINT('Ctrl Pts',(90.8711511133492,-1.95385585989427,-1.02259582539034));
#9530=CARTESIAN_POINT('Ctrl Pts',(90.875206354581,-1.91678970801654,-1.08790312769193));
#9531=CARTESIAN_POINT('Ctrl Pts',(90.8792602957455,-1.87973543915321,-1.15318949316639));
#9532=CARTESIAN_POINT('Ctrl Pts',(90.88331423691,-1.8393286859202,-1.21660385243824));
#9533=CARTESIAN_POINT('Ctrl Pts',(90.8873681780745,-1.79579288744773,-1.2777886779089));
#9534=CARTESIAN_POINT('Ctrl Pts',(90.8914221373556,-1.75225689441882,-1.33897377680743));
#9535=CARTESIAN_POINT('Ctrl Pts',(90.8954760966367,-1.70559210734747,-1.39792893317653));
#9536=CARTESIAN_POINT('Ctrl Pts',(90.8995300559178,-1.65606433175256,-1.45432696774038));
#9537=CARTESIAN_POINT('Ctrl Pts',(90.903588151952,-1.6064860168781,-1.51078255215382));
#9538=CARTESIAN_POINT('Ctrl Pts',(90.9076462479862,-1.55403919597851,-1.5646754435487));
#9539=CARTESIAN_POINT('Ctrl Pts',(90.9117043440205,-1.49902838264026,-1.61571343623767));
#9540=CARTESIAN_POINT('Ctrl Pts',(90.9157645471804,-1.44398900548803,-1.66677792989327));
#9541=CARTESIAN_POINT('Ctrl Pts',(90.9198247503404,-1.38638335227213,-1.71498426556534));
#9542=CARTESIAN_POINT('Ctrl Pts',(90.9238849535004,-1.32654899637501,-1.76008061185176));
#9543=CARTESIAN_POINT('Ctrl Pts',(90.9279524456706,-1.26660722387395,-1.80525791658245));
#9544=CARTESIAN_POINT('Ctrl Pts',(90.9320199378409,-1.20442915406587,-1.8473138115681));
#9545=CARTESIAN_POINT('Ctrl Pts',(90.9360874300111,-1.14038090942948,-1.88604013250217));
#9546=CARTESIAN_POINT('Ctrl Pts',(90.9392661129335,-1.09032818580747,-1.91630416002727));
#9547=CARTESIAN_POINT('Ctrl Pts',(90.9424447958558,-1.0391339147687,-1.94453563114969));
#9548=CARTESIAN_POINT('Ctrl Pts',(90.9456234787781,-0.986981606041235,-1.97065555319449));
#9549=CARTESIAN_POINT('Ctrl Pts',(90.949697228417,-0.920144033992175,-2.00413043118519));
#9550=CARTESIAN_POINT('Ctrl Pts',(90.9537709780558,-0.851472863040309,-2.03426555142575));
#9551=CARTESIAN_POINT('Ctrl Pts',(90.9578447276947,-0.781335344783656,-2.06085687979341));
#9552=CARTESIAN_POINT('Ctrl Pts',(90.9619124935517,-0.711300848961369,-2.08740914913175));
#9553=CARTESIAN_POINT('Ctrl Pts',(90.9659802594088,-0.639804724761734,-2.11042779364493));
#9554=CARTESIAN_POINT('Ctrl Pts',(90.9700480252658,-0.567237476967494,-2.1297553016071));
#9555=CARTESIAN_POINT('Ctrl Pts',(90.9741110298079,-0.494755169047744,-2.14906018674492));
#9556=CARTESIAN_POINT('Ctrl Pts',(90.97817403435,-0.42120468736276,-2.16468239700842));
#9557=CARTESIAN_POINT('Ctrl Pts',(90.9822370388921,-0.346993562062258,-2.1765136038829));
#9558=CARTESIAN_POINT('Ctrl Pts',(90.9862974630882,-0.27282956700218,-2.18833729695643));
#9559=CARTESIAN_POINT('Ctrl Pts',(90.9903578872843,-0.198006231046259,-2.19637468937789));
#9560=CARTESIAN_POINT('Ctrl Pts',(90.9944183114804,-0.122941882356516,-2.20056840238213));
#9561=CARTESIAN_POINT('Ctrl Pts',(90.9984774678744,-0.0479009713020453,
-2.20476080596695));
#9562=CARTESIAN_POINT('Ctrl Pts',(91.0025366242683,0.0273803268527341,-2.20511188635905));
#9563=CARTESIAN_POINT('Ctrl Pts',(91.0065957806623,0.102479553979722,-2.20161621110858));
#9564=CARTESIAN_POINT('Ctrl Pts',(91.0106549801117,0.177579577683765,-2.19812049877951));
#9565=CARTESIAN_POINT('Ctrl Pts',(91.0147141795611,0.25249704984926,-2.19077797377606));
#9566=CARTESIAN_POINT('Ctrl Pts',(91.0187733790105,0.326812124591935,-2.17963525279339));
#9567=CARTESIAN_POINT('Ctrl Pts',(91.022836717627,0.401202978441364,-2.16848116957438));
#9568=CARTESIAN_POINT('Ctrl Pts',(91.0269000562434,0.474989735164241,-2.15351922299617));
#9569=CARTESIAN_POINT('Ctrl Pts',(91.0309633948599,0.547761015715058,-2.1348475050136));
#9570=CARTESIAN_POINT('Ctrl Pts',(91.0350288503013,0.620570206977919,-2.11616605986781));
#9571=CARTESIAN_POINT('Ctrl Pts',(91.0390943057426,0.692362412501551,-2.09377113684108));
#9572=CARTESIAN_POINT('Ctrl Pts',(91.043159761184,0.762742296738048,-2.06781048183018));
#9573=CARTESIAN_POINT('Ctrl Pts',(91.0472324618394,0.833247607837265,-2.04180356127697));
#9574=CARTESIAN_POINT('Ctrl Pts',(91.0513051624947,0.902335130804898,-2.01221840394449));
#9575=CARTESIAN_POINT('Ctrl Pts',(91.0553778631501,0.969630779096078,-1.97925040159893));
#9576=CARTESIAN_POINT('Ctrl Pts',(91.0585099736992,1.02138449923315,-1.95389635850409));
#9577=CARTESIAN_POINT('Ctrl Pts',(91.0616420842482,1.07207886378984,-1.92654256107378));
#9578=CARTESIAN_POINT('Ctrl Pts',(91.0647741947973,1.12155540262169,-1.89729530617933));
#9579=CARTESIAN_POINT('Ctrl Pts',(91.0688479806445,1.18590716176332,-1.85925480563181));
#9580=CARTESIAN_POINT('Ctrl Pts',(91.0729217664916,1.24844494575908,-1.8178635523109));
#9581=CARTESIAN_POINT('Ctrl Pts',(91.0769955523388,1.30879830848776,-1.77331976465035));
#9582=CARTESIAN_POINT('Ctrl Pts',(91.0810633696527,1.3690632470665,-1.72884123841652));
#9583=CARTESIAN_POINT('Ctrl Pts',(91.0851311869666,1.42714973775237,-1.68121962924715));
#9584=CARTESIAN_POINT('Ctrl Pts',(91.0891990042805,1.48271384986785,-1.63069789949275));
#9585=CARTESIAN_POINT('Ctrl Pts',(91.0932620830264,1.53821323579128,-1.58023502209931));
#9586=CARTESIAN_POINT('Ctrl Pts',(91.0973251617723,1.59119572955431,-1.52687905559947));
#9587=CARTESIAN_POINT('Ctrl Pts',(91.1013882405182,1.64134952364412,-1.47091391360379));
#9588=CARTESIAN_POINT('Ctrl Pts',(91.1054487528421,1.69147163835721,-1.41498412169177));
#9589=CARTESIAN_POINT('Ctrl Pts',(91.109509265166,1.73876828130666,-1.35644877928074));
#9590=CARTESIAN_POINT('Ctrl Pts',(91.1135697774898,1.7829646278059,-1.29562847143499));
#9591=CARTESIAN_POINT('Ctrl Pts',(91.1176290358398,1.82714732551904,-1.23482694621355));
#9592=CARTESIAN_POINT('Ctrl Pts',(91.1216882941898,1.86823134738425,-1.1717422424517));
#9593=CARTESIAN_POINT('Ctrl Pts',(91.1257475525398,1.9059833003935,-1.10672655096962));
#9594=CARTESIAN_POINT('Ctrl Pts',(91.1298068676916,1.94373578167153,-1.04170994971314));
#9595=CARTESIAN_POINT('Ctrl Pts',(91.1338661828434,1.97815586340892,-0.974762720713493));
#9596=CARTESIAN_POINT('Ctrl Pts',(91.1379254979952,2.00905532200643,-0.906263048522695));
#9597=CARTESIAN_POINT('Ctrl Pts',(91.1419889730131,2.03998644545502,-0.837693179894235));
#9598=CARTESIAN_POINT('Ctrl Pts',(91.146052448031,2.06738954448393,-0.767568127170326));
#9599=CARTESIAN_POINT('Ctrl Pts',(91.1501159230489,2.09112425233576,-0.696286838374254));
#9600=CARTESIAN_POINT('Ctrl Pts',(91.1541815265921,2.11487139287808,-0.624968211086075));
#9601=CARTESIAN_POINT('Ctrl Pts',(91.1582471301353,2.13494618808701,-0.552492601980794));
#9602=CARTESIAN_POINT('Ctrl Pts',(91.1623127336786,2.15125870146638,-0.47927236449139));
#9603=CARTESIAN_POINT('Ctrl Pts',(91.1663856001343,2.1676003559943,-0.40592132423925));
#9604=CARTESIAN_POINT('Ctrl Pts',(91.17045846659,2.18016622400246,-0.331823469819038));
#9605=CARTESIAN_POINT('Ctrl Pts',(91.1745313330457,2.18891792995835,-0.2573990984966));
#9606=CARTESIAN_POINT('Ctrl Pts',(91.1776625256359,2.19564618317733,-0.20018213777551));
#9607=CARTESIAN_POINT('Ctrl Pts',(91.1807937182261,2.20012116454199,-0.142772367545864));
#9608=CARTESIAN_POINT('Ctrl Pts',(91.1839249108164,2.20234638625319,-0.0853603828337333));
#9609=CARTESIAN_POINT('Ctrl Pts',(91.187997411325,2.20524056037039,-0.0106890458901615));
#9610=CARTESIAN_POINT('Ctrl Pts',(91.1920699118336,2.20433838784057,0.0642740422392719));
#9611=CARTESIAN_POINT('Ctrl Pts',(91.1961424123423,2.19960548666169,0.139110398776636));
#9612=CARTESIAN_POINT('Ctrl Pts',(91.2002089201829,2.19487954992769,0.213836633918954));
#9613=CARTESIAN_POINT('Ctrl Pts',(91.2042754280235,2.18633410587648,0.288436035025831));
#9614=CARTESIAN_POINT('Ctrl Pts',(91.2083419358642,2.17398674374528,0.362488121211967));
#9615=CARTESIAN_POINT('Ctrl Pts',(91.2124036752274,2.16165386040528,0.43645337227642));
#9616=CARTESIAN_POINT('Ctrl Pts',(91.2164654145906,2.14552799453576,0.509872114776402));
#9617=CARTESIAN_POINT('Ctrl Pts',(91.2205271539538,2.12567856202451,0.582328645139008));
#9618=CARTESIAN_POINT('Ctrl Pts',(91.2245863092188,2.10584175781765,0.654739078308608));
#9619=CARTESIAN_POINT('Ctrl Pts',(91.2286454644839,2.08228621371744,0.726188054632568));
#9620=CARTESIAN_POINT('Ctrl Pts',(91.232704619749,2.0551322121439,0.796271053478975));
#9621=CARTESIAN_POINT('Ctrl Pts',(91.2367625053054,2.02798670437495,0.866332130278421));
#9622=CARTESIAN_POINT('Ctrl Pts',(91.2408203908618,1.99724514638297,0.935027632873771));
#9623=CARTESIAN_POINT('Ctrl Pts',(91.2448782764182,1.96307684258466,1.00197071319866));
#9624=CARTESIAN_POINT('Ctrl Pts',(91.2489362049661,1.92890817678793,1.06891450275659));
#9625=CARTESIAN_POINT('Ctrl Pts',(91.2529941335141,1.89131291182923,1.13410540859003));
#9626=CARTESIAN_POINT('Ctrl Pts',(91.257052062062,1.85050668370051,1.19718044319967));
#9627=CARTESIAN_POINT('Ctrl Pts',(91.2611141386116,1.80965874357502,1.26031995290932));
#9628=CARTESIAN_POINT('Ctrl Pts',(91.2651762151612,1.76559354584184,1.32133887042383));
#9629=CARTESIAN_POINT('Ctrl Pts',(91.2692382917108,1.71857011781289,1.37990316695071));
#9630=CARTESIAN_POINT('Ctrl Pts',(91.2733024880002,1.67152215124388,1.43849802446381));
#9631=CARTESIAN_POINT('Ctrl Pts',(91.2773666842895,1.62151319824356,1.49463535323905));
#9632=CARTESIAN_POINT('Ctrl Pts',(91.2814308805788,1.56884088670155,1.5480162377099));
#9633=CARTESIAN_POINT('Ctrl Pts',(91.2855023412743,1.51607442787032,1.60149253598397));
#9634=CARTESIAN_POINT('Ctrl Pts',(91.2895738019698,1.46063545467096,1.65220222600835));
#9635=CARTESIAN_POINT('Ctrl Pts',(91.2936452626652,1.40285621719685,1.69988541786561));
#9636=CARTESIAN_POINT('Ctrl Pts',(91.2967887173887,1.35824657202552,1.73670020397874));
#9637=CARTESIAN_POINT('Ctrl Pts',(91.2999321721121,1.312242636158,1.7717117089801));
#9638=CARTESIAN_POINT('Ctrl Pts',(91.3030756268355,1.26500851005774,1.80481840346377));
#9639=CARTESIAN_POINT('Ctrl Pts',(91.3071951970518,1.20310709387826,1.84820549332355));
#9640=CARTESIAN_POINT('Ctrl Pts',(91.3113147672681,1.13885577516707,1.8884852462642));
#9641=CARTESIAN_POINT('Ctrl Pts',(91.3154343374845,1.07259506399885,1.9253975767839));
#9642=CARTESIAN_POINT('Ctrl Pts',(91.3195475167814,1.00643714677331,1.96225264314328));
#9643=CARTESIAN_POINT('Ctrl Pts',(91.3236606960783,0.938276428746113,1.9957504383066));
#9644=CARTESIAN_POINT('Ctrl Pts',(91.3277738753752,0.868483277122665,2.02567341823856));
#9645=CARTESIAN_POINT('Ctrl Pts',(91.3318810969693,0.798791216850553,2.05555305646138));
#9646=CARTESIAN_POINT('Ctrl Pts',(91.3359883185635,0.727471847580355,2.08186799348214));
#9647=CARTESIAN_POINT('Ctrl Pts',(91.3400955401576,0.654919597791209,2.10444679676845));
#9648=CARTESIAN_POINT('Ctrl Pts',(91.344199215925,0.582429983460193,2.12700610743129));
#9649=CARTESIAN_POINT('Ctrl Pts',(91.3483028916924,0.508710043147842,2.14583555337324));
#9650=CARTESIAN_POINT('Ctrl Pts',(91.3524065674598,0.434172636937849,2.16081237531962));
#9651=CARTESIAN_POINT('Ctrl Pts',(91.356508427657,0.359668207966178,2.17578257114026));
#9652=CARTESIAN_POINT('Ctrl Pts',(91.3606102878542,0.284347483751757,2.18690343172747));
#9653=CARTESIAN_POINT('Ctrl Pts',(91.3647121480514,0.208635661003606,2.19410281458221));
#9654=CARTESIAN_POINT('Ctrl Pts',(91.3684909009685,0.138887727795815,2.20073509546337));
#9655=CARTESIAN_POINT('Ctrl Pts',(91.3722696538855,0.0688082964965979,2.20403987268341));
#9656=CARTESIAN_POINT('Ctrl Pts',(91.3760484068025,-0.00126552476430762,
2.20399963667127));
#9657=CARTESIAN_POINT('',(92.1260484067482,-0.00117773768617704,2.20399968532982));
#9658=CARTESIAN_POINT('Ctrl Pts',(91.3760484068552,-0.00126552574240776,
2.2039996366707));
#9659=CARTESIAN_POINT('Ctrl Pts',(91.3805750013567,-0.0852074454640055,
2.2039514376336));
#9660=CARTESIAN_POINT('Ctrl Pts',(91.3851015958581,-0.168975608381795,2.19910358289283));
#9661=CARTESIAN_POINT('Ctrl Pts',(91.3896281903595,-0.252053052579413,2.18953996508066));
#9662=CARTESIAN_POINT('Ctrl Pts',(91.3941731607358,-0.335467752682458,2.17993752341424));
#9663=CARTESIAN_POINT('Ctrl Pts',(91.3987181311122,-0.418185860182198,2.16558108788022));
#9664=CARTESIAN_POINT('Ctrl Pts',(91.4032631014886,-0.499701398972763,2.14660534609058));
#9665=CARTESIAN_POINT('Ctrl Pts',(91.4078314961518,-0.581637060052887,2.12753180537567));
#9666=CARTESIAN_POINT('Ctrl Pts',(91.412399890815,-0.662357477674704,2.10379135432718));
#9667=CARTESIAN_POINT('Ctrl Pts',(91.4169682854782,-0.741370049144116,2.07556894615237));
#9668=CARTESIAN_POINT('Ctrl Pts',(91.4187209712703,-0.771683588499686,2.06474128841378));
#9669=CARTESIAN_POINT('Ctrl Pts',(91.4204736570625,-0.801745989238771,2.05325441876248));
#9670=CARTESIAN_POINT('Ctrl Pts',(91.4222263428546,-0.8315303725407,2.04112058427285));
#9671=CARTESIAN_POINT('Ctrl Pts',(91.4262994818301,-0.900747532304323,2.01292226464003));
#9672=CARTESIAN_POINT('Ctrl Pts',(91.4303726208057,-0.968662122249928,1.98114472878017));
#9673=CARTESIAN_POINT('Ctrl Pts',(91.4344457597813,-1.03487872486445,1.94592960428247));
#9674=CARTESIAN_POINT('Ctrl Pts',(91.4385129163849,-1.10099807267219,1.91076620155836));
#9675=CARTESIAN_POINT('Ctrl Pts',(91.4425800729885,-1.16542396652118,1.87217545668805));
#9676=CARTESIAN_POINT('Ctrl Pts',(91.4466472295922,-1.22778064353879,1.83034715050218));
#9677=CARTESIAN_POINT('Ctrl Pts',(91.4507096300371,-1.29006440026404,1.78856775860204));
#9678=CARTESIAN_POINT('Ctrl Pts',(91.4547720304821,-1.350283353155,1.74355859198948));
#9679=CARTESIAN_POINT('Ctrl Pts',(91.4588344309271,-1.40808750137832,1.69555465510911));
#9680=CARTESIAN_POINT('Ctrl Pts',(91.4628942545007,-1.46585498313863,1.64758116819868));
#9681=CARTESIAN_POINT('Ctrl Pts',(91.4669540780743,-1.52121033348808,1.59661698492927));
#9682=CARTESIAN_POINT('Ctrl Pts',(91.4710139016479,-1.57383474947358,1.54293881322281));
#9683=CARTESIAN_POINT('Ctrl Pts',(91.4750724617826,-1.62644278845851,1.48927734645136));
#9684=CARTESIAN_POINT('Ctrl Pts',(91.4791310219174,-1.67632124646478,1.43290390888715));
#9685=CARTESIAN_POINT('Ctrl Pts',(91.4831895820521,-1.72318766461713,1.37413255274422));
#9686=CARTESIAN_POINT('Ctrl Pts',(91.4872481904981,-1.77005464064554,1.31536049701439));
#9687=CARTESIAN_POINT('Ctrl Pts',(91.491306798944,-1.8139092093616,1.25419084043354));
#9688=CARTESIAN_POINT('Ctrl Pts',(91.4953654073899,-1.85450977849573,1.19096997504711));
#9689=CARTESIAN_POINT('Ctrl Pts',(91.4994281673881,-1.89515187796876,1.12768444101142));
#9690=CARTESIAN_POINT('Ctrl Pts',(91.5034909273863,-1.93253307243781,1.06234391084669));
#9691=CARTESIAN_POINT('Ctrl Pts',(91.5075536873845,-1.96645606353663,0.995322334814222));
#9692=CARTESIAN_POINT('Ctrl Pts',(91.511618570171,-2.00039677936625,0.928265740071575));
#9693=CARTESIAN_POINT('Ctrl Pts',(91.5156834529574,-2.03087549983843,0.859526787188141));
#9694=CARTESIAN_POINT('Ctrl Pts',(91.5197483357439,-2.05774284607534,0.789500081966922));
#9695=CARTESIAN_POINT('Ctrl Pts',(91.5238204801591,-2.08465818894722,0.71934827893443));
#9696=CARTESIAN_POINT('Ctrl Pts',(91.5278926245744,-2.10794912307746,0.647904583136306));
#9697=CARTESIAN_POINT('Ctrl Pts',(91.5319647689896,-2.12751610903421,0.575579017859356));
#9698=CARTESIAN_POINT('Ctrl Pts',(91.5351021989511,-2.14259171582389,0.519854963814099));
#9699=CARTESIAN_POINT('Ctrl Pts',(91.5382396289125,-2.15545777028684,0.463607753674997));
#9700=CARTESIAN_POINT('Ctrl Pts',(91.5413770588739,-2.16608968285123,0.407027622951379));
#9701=CARTESIAN_POINT('Ctrl Pts',(91.5454500518947,-2.17989196886407,0.333575631866891));
#9702=CARTESIAN_POINT('Ctrl Pts',(91.5495230449155,-2.1899805161034,0.259279095173511));
#9703=CARTESIAN_POINT('Ctrl Pts',(91.5535960379363,-2.19626008992354,0.184547060147347));
#9704=CARTESIAN_POINT('Ctrl Pts',(91.5576630456856,-2.20253043589715,0.109924843999052));
#9705=CARTESIAN_POINT('Ctrl Pts',(91.5617300534348,-2.20500288170145,0.034868871960869));
#9706=CARTESIAN_POINT('Ctrl Pts',(91.5657970611841,-2.2036333135183,-0.0402022331763572));
#9707=CARTESIAN_POINT('Ctrl Pts',(91.5698593091387,-2.20226534819985,-0.115185479361682));
#9708=CARTESIAN_POINT('Ctrl Pts',(91.5739215570934,-2.19706431102125,-0.190183348458034));
#9709=CARTESIAN_POINT('Ctrl Pts',(91.5779838050481,-2.188038056443,-0.264774363481676));
#9710=CARTESIAN_POINT('Ctrl Pts',(91.5820434739773,-2.17901753242112,-0.339318022427398));
#9711=CARTESIAN_POINT('Ctrl Pts',(91.5861031429065,-2.16617666738495,-0.413454867052116));
#9712=CARTESIAN_POINT('Ctrl Pts',(91.5901628118357,-2.14957527116945,-0.486767042410209));
#9713=CARTESIAN_POINT('Ctrl Pts',(91.5942212153926,-2.13297904950067,-0.560056366842309));
#9714=CARTESIAN_POINT('Ctrl Pts',(91.5982796189495,-2.1126247292547,-0.63252106697144));
#9715=CARTESIAN_POINT('Ctrl Pts',(91.6023380225064,-2.08862320050254,-0.703753597733288));
#9716=CARTESIAN_POINT('Ctrl Pts',(91.6063964726597,-2.06462139617726,-0.774986946350117));
#9717=CARTESIAN_POINT('Ctrl Pts',(91.6104549228131,-2.0369724543631,-0.844987645597734));
#9718=CARTESIAN_POINT('Ctrl Pts',(91.6145133729665,-2.00583658980416,-0.913364973601909));
#9719=CARTESIAN_POINT('Ctrl Pts',(91.618575973101,-1.97466888716769,-0.981812221060761));
#9720=CARTESIAN_POINT('Ctrl Pts',(91.6226385732356,-1.94000733987067,-1.04863234686805));
#9721=CARTESIAN_POINT('Ctrl Pts',(91.6267011733701,-1.90205932544707,-1.11345692439351));
#9722=CARTESIAN_POINT('Ctrl Pts',(91.6307658951693,-1.8640914929368,-1.17831535610383));
#9723=CARTESIAN_POINT('Ctrl Pts',(91.6348306169685,-1.8228340376301,-1.24117576461928));
#9724=CARTESIAN_POINT('Ctrl Pts',(91.6388953387677,-1.77853766264782,-1.30169880638465));
#9725=CARTESIAN_POINT('Ctrl Pts',(91.6429673221698,-1.73416215243794,-1.36232997222761));
#9726=CARTESIAN_POINT('Ctrl Pts',(91.6470393055718,-1.6867371803264,-1.42061505978353));
#9727=CARTESIAN_POINT('Ctrl Pts',(91.6511112889739,-1.63655341271886,-1.47624826073336));
#9728=CARTESIAN_POINT('Ctrl Pts',(91.6542501176136,-1.59786999202185,-1.51913229713918));
#9729=CARTESIAN_POINT('Ctrl Pts',(91.6573889462533,-1.55754816328923,-1.56044129681809));
#9730=CARTESIAN_POINT('Ctrl Pts',(91.660527774893,-1.5157347010061,-1.60005134797791));
#9731=CARTESIAN_POINT('Ctrl Pts',(91.6646008602942,-1.46147566926288,-1.6514511342161));
#9732=CARTESIAN_POINT('Ctrl Pts',(91.6686739456953,-1.40449453518078,-1.7001869538125));
#9733=CARTESIAN_POINT('Ctrl Pts',(91.6727470310965,-1.34508352594941,-1.74595713241176));
#9734=CARTESIAN_POINT('Ctrl Pts',(91.6768141325442,-1.28575980011181,-1.79166006797689));
#9735=CARTESIAN_POINT('Ctrl Pts',(91.6808812339918,-1.22401366180412,-1.83440572391679));
#9736=CARTESIAN_POINT('Ctrl Pts',(91.6849483354395,-1.16017308285962,-1.87393020622648));
#9737=CARTESIAN_POINT('Ctrl Pts',(91.6890106786162,-1.09640719366077,-1.91340844720221));
#9738=CARTESIAN_POINT('Ctrl Pts',(91.6930730217929,-1.03055213607067,-1.94967275180106));
#9739=CARTESIAN_POINT('Ctrl Pts',(91.6971353649696,-0.962966436641571,-1.98250135987389));
#9740=CARTESIAN_POINT('Ctrl Pts',(91.7011951300076,-0.895423630021125,-2.01530913349186));
#9741=CARTESIAN_POINT('Ctrl Pts',(91.7052548950456,-0.826152789483229,-2.04468532935635));
#9742=CARTESIAN_POINT('Ctrl Pts',(91.7093146600835,-0.755537546089829,-2.07045381896061));
#9743=CARTESIAN_POINT('Ctrl Pts',(91.7133731604978,-0.684944299464992,-2.09621428163648));
#9744=CARTESIAN_POINT('Ctrl Pts',(91.7174316609121,-0.613007929694532,-2.11836910575678));
#9745=CARTESIAN_POINT('Ctrl Pts',(91.7214901613263,-0.5401310772917,-2.13679068215483));
#9746=CARTESIAN_POINT('Ctrl Pts',(91.7255487089482,-0.467253377200514,-2.15521247282882));
#9747=CARTESIAN_POINT('Ctrl Pts',(91.7296072565701,-0.393435636091098,-2.16990081428895));
#9748=CARTESIAN_POINT('Ctrl Pts',(91.733665804192,-0.3190930785952,-2.18077866992335));
#9749=CARTESIAN_POINT('Ctrl Pts',(91.7377285020664,-0.244674498734269,-2.19166764920401));
#9750=CARTESIAN_POINT('Ctrl Pts',(91.7417911999409,-0.169730504251898,-2.19873829212051));
#9751=CARTESIAN_POINT('Ctrl Pts',(91.7458538978153,-0.0946831335760688,
-2.20196528224589));
#9752=CARTESIAN_POINT('Ctrl Pts',(91.749918717659,-0.0195965652486128,-2.20519395784584));
#9753=CARTESIAN_POINT('Ctrl Pts',(91.7539835375028,0.0555930089127864,-2.20457498672492));
#9754=CARTESIAN_POINT('Ctrl Pts',(91.7580483573465,0.130464520518895,-2.20013522513635));
#9755=CARTESIAN_POINT('Ctrl Pts',(91.7621204381796,0.205469775137128,-2.19568753279982));
#9756=CARTESIAN_POINT('Ctrl Pts',(91.7661925190127,0.280155357103372,-2.18740547012963));
#9757=CARTESIAN_POINT('Ctrl Pts',(91.7702645998458,0.354106731721911,-2.1753676522715));
#9758=CARTESIAN_POINT('Ctrl Pts',(91.7734025635346,0.41109399150345,-2.1660912560311));
#9759=CARTESIAN_POINT('Ctrl Pts',(91.7765405272233,0.467645376738735,-2.15458564351988));
#9760=CARTESIAN_POINT('Ctrl Pts',(91.7796784909121,0.523577371692799,-2.14090698907058));
#9761=CARTESIAN_POINT('Ctrl Pts',(91.7837515628427,0.596177013136447,-2.1231521171182));
#9762=CARTESIAN_POINT('Ctrl Pts',(91.7878246347732,0.668012507929734,-2.10166596546539));
#9763=CARTESIAN_POINT('Ctrl Pts',(91.7918977067038,0.738671967899062,-2.07653069417241));
#9764=CARTESIAN_POINT('Ctrl Pts',(91.7959647946945,0.809227618761578,-2.0514323502783));
#9765=CARTESIAN_POINT('Ctrl Pts',(91.8000318826852,0.878610219013585,-2.02269568939249));
#9766=CARTESIAN_POINT('Ctrl Pts',(91.8040989706759,0.94642026728458,-1.99045338495354));
#9767=CARTESIAN_POINT('Ctrl Pts',(91.808161300483,1.01415098295711,-1.95824880155825));
#9768=CARTESIAN_POINT('Ctrl Pts',(91.8122236302901,1.0803123728134,-1.9225469270248));
#9769=CARTESIAN_POINT('Ctrl Pts',(91.8162859600972,1.14452379342688,-1.88352894490097));
#9770=CARTESIAN_POINT('Ctrl Pts',(91.820345711826,1.20869446351587,-1.84453572477774));
#9771=CARTESIAN_POINT('Ctrl Pts',(91.8244054635548,1.27091721306682,-1.80223082053647));
#9772=CARTESIAN_POINT('Ctrl Pts',(91.8284652152836,1.33083614956635,-1.75684124012599));
#9773=CARTESIAN_POINT('Ctrl Pts',(91.8325237024687,1.3907364223348,-1.71146579779893));
#9774=CARTESIAN_POINT('Ctrl Pts',(91.8365821896538,1.4483339264722,-1.66300787509311));
#9775=CARTESIAN_POINT('Ctrl Pts',(91.8406406768389,1.5033032499452,-1.6117367460923));
#9776=CARTESIAN_POINT('Ctrl Pts',(91.8446992113313,1.55827321416192,-1.56046501945536));
#9777=CARTESIAN_POINT('Ctrl Pts',(91.8487577458237,1.61061458895495,-1.50638034839004));
#9778=CARTESIAN_POINT('Ctrl Pts',(91.8528162803161,1.66003764990204,-1.44978998510395));
#9779=CARTESIAN_POINT('Ctrl Pts',(91.8568789653094,1.7095112538365,-1.3931417491171));
#9780=CARTESIAN_POINT('Ctrl Pts',(91.8609416503026,1.75606026939359,-1.33398306421869));
#9781=CARTESIAN_POINT('Ctrl Pts',(91.8650043352959,1.79943475082582,-1.27265493261938));
#9782=CARTESIAN_POINT('Ctrl Pts',(91.8690691423759,1.84283188831269,-1.21129476712698));
#9783=CARTESIAN_POINT('Ctrl Pts',(91.873133949456,1.88305093396025,-1.14776330210772));
#9784=CARTESIAN_POINT('Ctrl Pts',(91.877198756536,1.91988631850551,-1.08242899259738));
#9785=CARTESIAN_POINT('Ctrl Pts',(91.8812708249458,1.95678750540418,-1.01697797054615));
#9786=CARTESIAN_POINT('Ctrl Pts',(91.8853428933555,1.9902927444986,-0.94971809914239));
#9787=CARTESIAN_POINT('Ctrl Pts',(91.8894149617653,2.02024350971191,-0.881040385831942));
#9788=CARTESIAN_POINT('Ctrl Pts',(91.8925530434872,2.04332464180943,-0.828114880864567));
#9789=CARTESIAN_POINT('Ctrl Pts',(91.8956911252092,2.06429580802403,-0.77434782608217));
#9790=CARTESIAN_POINT('Ctrl Pts',(91.8988292069312,2.08310478479363,-0.719923923459901));
#9791=CARTESIAN_POINT('Ctrl Pts',(91.902902262903,2.10751779310294,-0.649284717339446));
#9792=CARTESIAN_POINT('Ctrl Pts',(91.9069753188747,2.12838068918864,-0.577266087120647));
#9793=CARTESIAN_POINT('Ctrl Pts',(91.9110483748465,2.14553935622089,-0.504258734091213));
#9794=CARTESIAN_POINT('Ctrl Pts',(91.9151154465387,2.16267281312546,-0.431358646077604));
#9795=CARTESIAN_POINT('Ctrl Pts',(91.9191825182309,2.1761127379984,-0.357473180329287));
#9796=CARTESIAN_POINT('Ctrl Pts',(91.923249589923,2.18575418144706,-0.283009996796427));
#9797=CARTESIAN_POINT('Ctrl Pts',(91.9273119029999,2.1953843440717,-0.208633937776962));
#9798=CARTESIAN_POINT('Ctrl Pts',(91.9313742160768,2.2012247941891,-0.133681975061804));
#9799=CARTESIAN_POINT('Ctrl Pts',(91.9354365291537,2.20322157239273,-0.0585722028209135));
#9800=CARTESIAN_POINT('Ctrl Pts',(91.9394962638958,2.20521708324879,0.016489897531451));
#9801=CARTESIAN_POINT('Ctrl Pts',(91.943555998638,2.20337375058481,0.0917091325659119));
#9802=CARTESIAN_POINT('Ctrl Pts',(91.9476157333801,2.19768954064834,0.166663382075649));
#9803=CARTESIAN_POINT('Ctrl Pts',(91.9516742033463,2.19200710157932,0.241594280223914));
#9804=CARTESIAN_POINT('Ctrl Pts',(91.9557326733125,2.18248619710266,0.316259880969424));
#9805=CARTESIAN_POINT('Ctrl Pts',(91.9597911432787,2.16917683287236,0.390240781735893));
#9806=CARTESIAN_POINT('Ctrl Pts',(91.9638496603438,2.1558673141854,0.464222541058963));
#9807=CARTESIAN_POINT('Ctrl Pts',(91.967908177409,2.13876933475411,0.537519115024085));
#9808=CARTESIAN_POINT('Ctrl Pts',(91.9719666944742,2.11798415696202,0.609720518645964));
#9809=CARTESIAN_POINT('Ctrl Pts',(91.9760293618367,2.09717772395114,0.681995756451299));
#9810=CARTESIAN_POINT('Ctrl Pts',(91.9800920291992,2.07267669532325,0.753173127615016));
#9811=CARTESIAN_POINT('Ctrl Pts',(91.9841546965617,2.04463225312056,0.822857794214245));
#9812=CARTESIAN_POINT('Ctrl Pts',(91.9882194858703,2.01657316320282,0.892578857370496));
#9813=CARTESIAN_POINT('Ctrl Pts',(91.9922842751789,1.98496717502972,0.96080522973781));
#9814=CARTESIAN_POINT('Ctrl Pts',(91.9963490644875,1.95001258876522,1.02716449688313));
#9815=CARTESIAN_POINT('Ctrl Pts',(92.0004211150953,1.91499555997531,1.09364230756357));
#9816=CARTESIAN_POINT('Ctrl Pts',(92.0044931657031,1.87661822892308,1.15824593975784));
#9817=CARTESIAN_POINT('Ctrl Pts',(92.0085652163109,1.83512334000208,1.22063029905849));
#9818=CARTESIAN_POINT('Ctrl Pts',(92.0117034518574,1.80314418552858,1.26870848687107));
#9819=CARTESIAN_POINT('Ctrl Pts',(92.0148416874039,1.76931430283252,1.31546910416486));
#9820=CARTESIAN_POINT('Ctrl Pts',(92.0179799229504,1.73376065666336,1.36076816005014));
#9821=CARTESIAN_POINT('Ctrl Pts',(92.02200424305,1.68816839605315,1.41885745844422));
#9822=CARTESIAN_POINT('Ctrl Pts',(92.0260285631496,1.63955510766071,1.47477792474616));
#9823=CARTESIAN_POINT('Ctrl Pts',(92.0300528832492,1.58815718622276,1.52819264225719));
#9824=CARTESIAN_POINT('Ctrl Pts',(92.0340704250322,1.53684583627448,1.58151739131159));
#9825=CARTESIAN_POINT('Ctrl Pts',(92.0380879668152,1.48275950468375,1.6323444236848));
#9826=CARTESIAN_POINT('Ctrl Pts',(92.0421055085981,1.42617564392087,1.68036871926577));
#9827=CARTESIAN_POINT('Ctrl Pts',(92.0461192504473,1.36964530218518,1.72834759176061));
#9828=CARTESIAN_POINT('Ctrl Pts',(92.0501329922964,1.31062248584389,1.77352866761993));
#9829=CARTESIAN_POINT('Ctrl Pts',(92.0541467341455,1.24942149077193,1.81564367054697));
#9830=CARTESIAN_POINT('Ctrl Pts',(92.0581580516425,1.18825746189424,1.85773323546636));
#9831=CARTESIAN_POINT('Ctrl Pts',(92.0621693691395,1.12491826638348,1.89676012336794));
#9832=CARTESIAN_POINT('Ctrl Pts',(92.0661806866365,1.05974987830951,1.93249739855529));
#9833=CARTESIAN_POINT('Ctrl Pts',(92.0701909521499,0.994598580899787,1.96822530150268));
#9834=CARTESIAN_POINT('Ctrl Pts',(92.0742012176632,0.927619472836517,2.00066506916662));
#9835=CARTESIAN_POINT('Ctrl Pts',(92.0782114831766,0.859184460530739,2.02963495801154));
#9836=CARTESIAN_POINT('Ctrl Pts',(92.0822246038918,0.790700724323783,2.05862547264366));
#9837=CARTESIAN_POINT('Ctrl Pts',(92.0862377246071,0.720759463365022,2.0841409770544));
#9838=CARTESIAN_POINT('Ctrl Pts',(92.0902508453224,0.649753047421367,2.10604771488365));
#9839=CARTESIAN_POINT('Ctrl Pts',(92.0942652306258,0.578724256405135,2.12796135581937));
#9840=CARTESIAN_POINT('Ctrl Pts',(92.0982796159292,0.506630116881663,2.14626384139877));
#9841=CARTESIAN_POINT('Ctrl Pts',(92.1022940012325,0.43387604195787,2.16087194905551));
#9842=CARTESIAN_POINT('Ctrl Pts',(92.1063150631176,0.361000965064446,2.1755043523933));
#9843=CARTESIAN_POINT('Ctrl Pts',(92.1103361250028,0.287464245593512,2.18643002725376));
#9844=CARTESIAN_POINT('Ctrl Pts',(92.1143571868879,0.213678759559795,2.19361742054374));
#9845=CARTESIAN_POINT('Ctrl Pts',(92.1182542601747,0.142168433484382,2.20058319207182));
#9846=CARTESIAN_POINT('Ctrl Pts',(92.1221513334614,0.0704248760134409,2.20403794717584));
#9847=CARTESIAN_POINT('Ctrl Pts',(92.1260484067482,-0.00117773768617677,
2.20399968532982));
#9848=CARTESIAN_POINT('',(92.8760484068423,0.00195929737048231,2.20399912911821));
#9849=CARTESIAN_POINT('Ctrl Pts',(92.1260484068025,-0.00117773868358856,
2.20399968532929));
#9850=CARTESIAN_POINT('Ctrl Pts',(92.1297424841915,-0.0690506209188907,
2.2039634164861));
#9851=CARTESIAN_POINT('Ctrl Pts',(92.1334365615805,-0.1368377559261,2.2007921759398));
#9852=CARTESIAN_POINT('Ctrl Pts',(92.1371306389695,-0.204330579702541,2.19450792074178));
#9853=CARTESIAN_POINT('Ctrl Pts',(92.141203704471,-0.27874772454576,2.18757894217584));
#9854=CARTESIAN_POINT('Ctrl Pts',(92.1452767699724,-0.352955528673427,2.17684701259296));
#9855=CARTESIAN_POINT('Ctrl Pts',(92.1493498354739,-0.426534513105433,2.16233307081262));
#9856=CARTESIAN_POINT('Ctrl Pts',(92.1534169168641,-0.500005395954242,2.1478404527852));
#9857=CARTESIAN_POINT('Ctrl Pts',(92.1574839982543,-0.572848828793578,2.12957694611157));
#9858=CARTESIAN_POINT('Ctrl Pts',(92.1615510796445,-0.644650186407671,2.10761527256863));
#9859=CARTESIAN_POINT('Ctrl Pts',(92.1656134026252,-0.716367537771774,2.08567929377437));
#9860=CARTESIAN_POINT('Ctrl Pts',(92.169675725606,-0.787044781913827,2.06005388339878));
#9861=CARTESIAN_POINT('Ctrl Pts',(92.1737380485868,-0.856278842209428,2.03086251242778));
#9862=CARTESIAN_POINT('Ctrl Pts',(92.1777977933541,-0.925468962083327,2.00168966819269));
#9863=CARTESIAN_POINT('Ctrl Pts',(92.1818575381215,-0.993217276852615,1.96895553944629));
#9864=CARTESIAN_POINT('Ctrl Pts',(92.1859172828888,-1.05913848129819,1.93283255286985));
#9865=CARTESIAN_POINT('Ctrl Pts',(92.1899757629871,-1.12503915033849,1.89672081912434));
#9866=CARTESIAN_POINT('Ctrl Pts',(92.1940342430855,-1.18911342067678,1.85722255284776));
#9867=CARTESIAN_POINT('Ctrl Pts',(92.1980927231838,-1.25099994751136,1.81455645581133));
#9868=CARTESIAN_POINT('Ctrl Pts',(92.2021512504738,-1.31288719395815,1.77188986265651));
#9869=CARTESIAN_POINT('Ctrl Pts',(92.2062097777639,-1.37258625431501,1.72605563808882));
#9870=CARTESIAN_POINT('Ctrl Pts',(92.2102683050539,-1.42976552330211,1.67731527995683));
#9871=CARTESIAN_POINT('Ctrl Pts',(92.2143309827146,-1.48700326550853,1.62852507848648));
#9872=CARTESIAN_POINT('Ctrl Pts',(92.2183936603752,-1.54171570642555,1.57682311916356));
#9873=CARTESIAN_POINT('Ctrl Pts',(92.2224563380358,-1.59360564660085,1.52251011265012));
#9874=CARTESIAN_POINT('Ctrl Pts',(92.2265211376994,-1.64552268973992,1.46816873756577));
#9875=CARTESIAN_POINT('Ctrl Pts',(92.230585937363,-1.69461398432032,1.41121396142467));
#9876=CARTESIAN_POINT('Ctrl Pts',(92.2346507370266,-1.74062220736324,1.35198015193786));
#9877=CARTESIAN_POINT('Ctrl Pts',(92.2387227979655,-1.78671261855897,1.29264052837992));
#9878=CARTESIAN_POINT('Ctrl Pts',(92.2427948589044,-1.82970868373798,1.23101413168966));
#9879=CARTESIAN_POINT('Ctrl Pts',(92.2468669198433,-1.86939631216582,1.16746452967995));
#9880=CARTESIAN_POINT('Ctrl Pts',(92.2500050648918,-1.89998169300921,1.1184898527615));
#9881=CARTESIAN_POINT('Ctrl Pts',(92.2531432099402,-1.92860305751758,1.06837358672696));
#9882=CARTESIAN_POINT('Ctrl Pts',(92.2562813549886,-1.95518168535522,1.01729080269682));
#9883=CARTESIAN_POINT('Ctrl Pts',(92.260354418832,-1.98967864020635,0.950989392965538));
#9884=CARTESIAN_POINT('Ctrl Pts',(92.2644274826753,-2.02086581555238,0.882803416388159));
#9885=CARTESIAN_POINT('Ctrl Pts',(92.2685005465187,-2.04853352782865,0.813096787204264));
#9886=CARTESIAN_POINT('Ctrl Pts',(92.2725676262122,-2.07616059067158,0.743492571076739));
#9887=CARTESIAN_POINT('Ctrl Pts',(92.2766347059057,-2.10027828190842,0.672372578128671));
#9888=CARTESIAN_POINT('Ctrl Pts',(92.2807017855992,-2.12072307109084,0.600124700160767));
#9889=CARTESIAN_POINT('Ctrl Pts',(92.2847641068334,-2.14114393999043,0.527961351784204));
#9890=CARTESIAN_POINT('Ctrl Pts',(92.2888264280676,-2.1579003151836,0.4546731972809));
#9891=CARTESIAN_POINT('Ctrl Pts',(92.2928887493018,-2.17087757788415,0.380665918936582));
#9892=CARTESIAN_POINT('Ctrl Pts',(92.2969484922929,-2.18384660427429,0.306705610968948));
#9893=CARTESIAN_POINT('Ctrl Pts',(92.301008235284,-2.1930411954764,0.232027553946412));
#9894=CARTESIAN_POINT('Ctrl Pts',(92.3050679782751,-2.19839750858312,0.157049018639201));
#9895=CARTESIAN_POINT('Ctrl Pts',(92.3091264565699,-2.20375215308451,0.0820938407387217));
#9896=CARTESIAN_POINT('Ctrl Pts',(92.3131849348648,-2.20527085951197,0.00683884633960688));
#9897=CARTESIAN_POINT('Ctrl Pts',(92.3172434131597,-2.20294166114478,-0.0682937595442691));
#9898=CARTESIAN_POINT('Ctrl Pts',(92.3213019386216,-2.20061243570799,-0.143427238608045));
#9899=CARTESIAN_POINT('Ctrl Pts',(92.3253604640835,-2.19443523327064,-0.218437849156203));
#9900=CARTESIAN_POINT('Ctrl Pts',(92.3294189895454,-2.18445017045167,-0.292905194241523));
#9901=CARTESIAN_POINT('Ctrl Pts',(92.3334816653521,-2.17445489666966,-0.367448691407455));
#9902=CARTESIAN_POINT('Ctrl Pts',(92.3375443411588,-2.16064404998701,-0.441447339419365));
#9903=CARTESIAN_POINT('Ctrl Pts',(92.3416070169655,-2.14310934695328,-0.514488412893325));
#9904=CARTESIAN_POINT('Ctrl Pts',(92.3456718147579,-2.1255654853278,-0.587567636621174));
#9905=CARTESIAN_POINT('Ctrl Pts',(92.3497366125503,-2.10429402923873,-0.659687831422038));
#9906=CARTESIAN_POINT('Ctrl Pts',(92.3538014103427,-2.0794365896898,-0.730451551753623));
#9907=CARTESIAN_POINT('Ctrl Pts',(92.3578734694033,-2.05453474534072,-0.801341682886763));
#9908=CARTESIAN_POINT('Ctrl Pts',(92.3619455284638,-2.02603430355675,-0.870870057001498));
#9909=CARTESIAN_POINT('Ctrl Pts',(92.3660175875243,-1.99412484198433,-0.938659743773515));
#9910=CARTESIAN_POINT('Ctrl Pts',(92.3691557486855,-1.96953358937916,-0.990902346101763));
#9911=CARTESIAN_POINT('Ctrl Pts',(92.3722939098467,-1.94291867194688,-1.04211273039333));
#9912=CARTESIAN_POINT('Ctrl Pts',(92.3754320710079,-1.91438458534593,-1.09212987295006));
#9913=CARTESIAN_POINT('Ctrl Pts',(92.3795051363958,-1.87734977593337,-1.1570478557071));
#9914=CARTESIAN_POINT('Ctrl Pts',(92.3835782017837,-1.83693769024174,-1.220205082403));
#9915=CARTESIAN_POINT('Ctrl Pts',(92.3876512671716,-1.79334058564205,-1.28122813889214));
#9916=CARTESIAN_POINT('Ctrl Pts',(92.3917183484339,-1.74980753367201,-1.34216154063763));
#9917=CARTESIAN_POINT('Ctrl Pts',(92.3957854296962,-1.70309902859019,-1.40096661217287));
#9918=CARTESIAN_POINT('Ctrl Pts',(92.3998525109586,-1.65345248745313,-1.45729573928392));
#9919=CARTESIAN_POINT('Ctrl Pts',(92.4039148337905,-1.60386403210157,-1.51355896207375));
#9920=CARTESIAN_POINT('Ctrl Pts',(92.4079771566225,-1.55134468426143,-1.56735163936944));
#9921=CARTESIAN_POINT('Ctrl Pts',(92.4120394794544,-1.49617331510964,-1.61835762770589));
#9922=CARTESIAN_POINT('Ctrl Pts',(92.4160992240601,-1.44103696145939,-1.66933124417464));
#9923=CARTESIAN_POINT('Ctrl Pts',(92.4201589686658,-1.38325227623498,-1.71752135802385));
#9924=CARTESIAN_POINT('Ctrl Pts',(92.4242187132716,-1.32313538205734,-1.76264822376672));
#9925=CARTESIAN_POINT('Ctrl Pts',(92.4282771931957,-1.26303721534587,-1.80776103170001));
#9926=CARTESIAN_POINT('Ctrl Pts',(92.4323356731198,-1.20060866376322,-1.84981219971173));
#9927=CARTESIAN_POINT('Ctrl Pts',(92.4363941530439,-1.1361981046941,-1.88856291049293));
#9928=CARTESIAN_POINT('Ctrl Pts',(92.4404526801473,-1.07178679686028,-1.92731407174631));
#9929=CARTESIAN_POINT('Ctrl Pts',(92.4445112072507,-1.00539384584266,-1.96276445498689));
#9930=CARTESIAN_POINT('Ctrl Pts',(92.4485697343542,-0.937394329159364,-1.99471999831051));
#9931=CARTESIAN_POINT('Ctrl Pts',(92.4526324118101,-0.869325274449837,-2.02670822018124));
#9932=CARTESIAN_POINT('Ctrl Pts',(92.456695089266,-0.799646806351258,-2.05519426171501));
#9933=CARTESIAN_POINT('Ctrl Pts',(92.460757766722,-0.728755512362739,-2.08003158706807));
#9934=CARTESIAN_POINT('Ctrl Pts',(92.4648225661705,-0.657827190871765,-2.10488188529938));
#9935=CARTESIAN_POINT('Ctrl Pts',(92.468887365619,-0.58568524050643,-2.12607953745661));
#9936=CARTESIAN_POINT('Ctrl Pts',(92.4729521650675,-0.512740439975553,-2.14352822263055));
#9937=CARTESIAN_POINT('Ctrl Pts',(92.4770242257767,-0.439665332595621,-2.16100807771884));
#9938=CARTESIAN_POINT('Ctrl Pts',(92.4810962864858,-0.365784980496466,-2.1747255016663));
#9939=CARTESIAN_POINT('Ctrl Pts',(92.4851683471949,-0.291518908767242,-2.18463560481632));
#9940=CARTESIAN_POINT('Ctrl Pts',(92.4883064938056,-0.234285523036974,-2.19227285750796));
#9941=CARTESIAN_POINT('Ctrl Pts',(92.4914446404162,-0.176823250123836,-2.19764997578432));
#9942=CARTESIAN_POINT('Ctrl Pts',(92.4945827870269,-0.119324044631328,-2.20076754164833));
#9943=CARTESIAN_POINT('Ctrl Pts',(92.4986558519924,-0.0446946443849952,
-2.20481389443992));
#9944=CARTESIAN_POINT('Ctrl Pts',(92.502728916958,0.0302847283983598,-2.20506765315536));
#9945=CARTESIAN_POINT('Ctrl Pts',(92.5068019819235,0.10519605238616,-2.2014880854918));
#9946=CARTESIAN_POINT('Ctrl Pts',(92.51086906276,0.179997316987484,-2.19791377691325));
#9947=CARTESIAN_POINT('Ctrl Pts',(92.5149361435965,0.254730258330918,-2.19051734618733));
#9948=CARTESIAN_POINT('Ctrl Pts',(92.5190032244329,0.328974071322962,-2.1793099963973));
#9949=CARTESIAN_POINT('Ctrl Pts',(92.5230655468359,0.403131019985645,-2.16811575906586));
#9950=CARTESIAN_POINT('Ctrl Pts',(92.5271278692388,0.476799507535252,-2.15311953205287));
#9951=CARTESIAN_POINT('Ctrl Pts',(92.5311901916418,0.549562719159225,-2.13438441188796));
#9952=CARTESIAN_POINT('Ctrl Pts',(92.5352499358168,0.622279750266912,-2.11566118231313));
#9953=CARTESIAN_POINT('Ctrl Pts',(92.5393096799918,0.694092184373747,-2.09320388721637));
#9954=CARTESIAN_POINT('Ctrl Pts',(92.5433694241668,0.764593615353688,-2.06712665392336));
#9955=CARTESIAN_POINT('Ctrl Pts',(92.5474279036591,0.835073083881017,-2.04105754415341));
#9956=CARTESIAN_POINT('Ctrl Pts',(92.5514863831514,0.904241912626709,-2.01137090066691));
#9957=CARTESIAN_POINT('Ctrl Pts',(92.5555448626437,0.971710619063381,-1.97823013646023));
#9958=CARTESIAN_POINT('Ctrl Pts',(92.5596033893149,1.0391801098077,-1.94508898700006));
#9959=CARTESIAN_POINT('Ctrl Pts',(92.563661915986,1.10494901124095,-1.90849384920838));
#9960=CARTESIAN_POINT('Ctrl Pts',(92.5677204426572,1.16865099081085,-1.86865482678766));
#9961=CARTESIAN_POINT('Ctrl Pts',(92.5717831196832,1.23241811367999,-1.82877506394762));
#9962=CARTESIAN_POINT('Ctrl Pts',(92.5758457967091,1.29411368805856,-1.78564504579));
#9963=CARTESIAN_POINT('Ctrl Pts',(92.5799084737351,1.35339967222153,-1.73951870562827));
#9964=CARTESIAN_POINT('Ctrl Pts',(92.5839732727543,1.41271662228537,-1.69336827303227));
#9965=CARTESIAN_POINT('Ctrl Pts',(92.5880380717735,1.46962111415404,-1.64421871423083));
#9966=CARTESIAN_POINT('Ctrl Pts',(92.5921028707926,1.52380962237535,-1.59236309764962));
#9967=CARTESIAN_POINT('Ctrl Pts',(92.5961749310783,1.57809493174209,-1.54041484734869));
#9968=CARTESIAN_POINT('Ctrl Pts',(92.600246991364,1.62965423832684,-1.48575123149518));
#9969=CARTESIAN_POINT('Ctrl Pts',(92.6043190516497,1.67822250537906,-1.42870053630537));
#9970=CARTESIAN_POINT('Ctrl Pts',(92.6074572021151,1.7156518456056,-1.38473417699251));
#9971=CARTESIAN_POINT('Ctrl Pts',(92.6105953525806,1.75130556742079,-1.33935084853213));
#9972=CARTESIAN_POINT('Ctrl Pts',(92.613733503046,1.78508015467132,-1.29271220362408));
#9973=CARTESIAN_POINT('Ctrl Pts',(92.617806567852,1.82891682986636,-1.23217902484069));
#9974=CARTESIAN_POINT('Ctrl Pts',(92.621879632658,1.86975547438596,-1.16929679093106));
#9975=CARTESIAN_POINT('Ctrl Pts',(92.625952697464,1.90733536041205,-1.10439477675414));
#9976=CARTESIAN_POINT('Ctrl Pts',(92.6300197781367,1.94486003419431,-1.03958811640106));
#9977=CARTESIAN_POINT('Ctrl Pts',(92.6340868588094,1.9791352178715,-0.972767977151691));
#9978=CARTESIAN_POINT('Ctrl Pts',(92.6381539394821,2.00994232671424,-0.904294113263235));
#9979=CARTESIAN_POINT('Ctrl Pts',(92.6422162617157,2.04071339158268,-0.835900363033059));
#9980=CARTESIAN_POINT('Ctrl Pts',(92.6462785839493,2.06802424824332,-0.765857165481326));
#9981=CARTESIAN_POINT('Ctrl Pts',(92.6503409061829,2.09170209012148,-0.694549037996206));
#9982=CARTESIAN_POINT('Ctrl Pts',(92.6544006501853,2.11536490439987,-0.62328616759172));
#9983=CARTESIAN_POINT('Ctrl Pts',(92.6584603941876,2.13539912935187,-0.550760412332747));
#9984=CARTESIAN_POINT('Ctrl Pts',(92.6625201381899,2.15168048912937,-0.477375190704345));
#9985=CARTESIAN_POINT('Ctrl Pts',(92.6665786175064,2.16795677696044,-0.404012829937562));
#9986=CARTESIAN_POINT('Ctrl Pts',(92.670637096823,2.18048241744174,-0.32979200020964));
#9987=CARTESIAN_POINT('Ctrl Pts',(92.6746955761395,2.189183728598,-0.255128599811503));
#9988=CARTESIAN_POINT('Ctrl Pts',(92.6787541026321,2.19788514089883,-0.180464331521415));
#9989=CARTESIAN_POINT('Ctrl Pts',(92.6828126291247,2.20276208212055,-0.10535795680518));
#9990=CARTESIAN_POINT('Ctrl Pts',(92.6868711556172,2.20379265668724,-0.0302312145207114));
#9991=CARTESIAN_POINT('Ctrl Pts',(92.6909338324614,2.20482428514549,0.0449723542663247));
#9992=CARTESIAN_POINT('Ctrl Pts',(92.6949965093056,2.20200168562654,0.120195853738261));
#9993=CARTESIAN_POINT('Ctrl Pts',(92.6990591861497,2.1953551296397,0.195017575527558));
#9994=CARTESIAN_POINT('Ctrl Pts',(92.703123984985,2.18870510206669,0.269878377715137));
#9995=CARTESIAN_POINT('Ctrl Pts',(92.7071887838203,2.17822720718454,0.344336511074202));
#9996=CARTESIAN_POINT('Ctrl Pts',(92.7112535826556,2.16400331096335,0.417978073754652));
#9997=CARTESIAN_POINT('Ctrl Pts',(92.7153256427561,2.1497540054939,0.491751188066224));
#9998=CARTESIAN_POINT('Ctrl Pts',(92.7193977028566,2.13174544698614,0.564704353817959));
#9999=CARTESIAN_POINT('Ctrl Pts',(92.7234697629571,2.11010995572858,0.63643693696638));
#10000=CARTESIAN_POINT('Ctrl Pts',(92.7266079149931,2.09343646386817,0.691717985453458));
#10001=CARTESIAN_POINT('Ctrl Pts',(92.7297460670292,2.07460994892254,0.746274379256409));
#10002=CARTESIAN_POINT('Ctrl Pts',(92.7328842190652,2.05371019199788,0.799931526622132));
#10003=CARTESIAN_POINT('Ctrl Pts',(92.7369572840645,2.02658401473007,0.869574120857797));
#10004=CARTESIAN_POINT('Ctrl Pts',(92.7410303490637,1.99585907533792,0.937969653685009));
#10005=CARTESIAN_POINT('Ctrl Pts',(92.745103414063,1.96167085979995,1.00472057698234));
#10006=CARTESIAN_POINT('Ctrl Pts',(92.7491704949322,1.92753287344565,1.07137343010157));
#10007=CARTESIAN_POINT('Ctrl Pts',(92.7532375758013,1.88994192900946,1.13638604950373));
#10008=CARTESIAN_POINT('Ctrl Pts',(92.7573046566705,1.84908196421617,1.1993797937311));
#10009=CARTESIAN_POINT('Ctrl Pts',(92.7613669791044,1.80826980508606,1.26229983604184));
#10010=CARTESIAN_POINT('Ctrl Pts',(92.7654293015382,1.76419648295336,1.3232052974903));
#10011=CARTESIAN_POINT('Ctrl Pts',(92.7694916239721,1.71709155235281,1.38174259572419));
#10012=CARTESIAN_POINT('Ctrl Pts',(92.773551368177,1.67001651777894,1.4402427421651));
#10013=CARTESIAN_POINT('Ctrl Pts',(92.7776111123818,1.61991399141386,1.49637733689366));
#10014=CARTESIAN_POINT('Ctrl Pts',(92.7816708565866,1.56705570899619,1.54982334635353));
#10015=CARTESIAN_POINT('Ctrl Pts',(92.7857293361077,1.51421389289049,1.60325270641382));
#10016=CARTESIAN_POINT('Ctrl Pts',(92.7897878156287,1.45861836070841,1.6539948048556));
#10017=CARTESIAN_POINT('Ctrl Pts',(92.7938462951497,1.40057875018951,1.70176237016735));
#10018=CARTESIAN_POINT('Ctrl Pts',(92.7979048218484,1.34253846499085,1.74953049075177));
#10019=CARTESIAN_POINT('Ctrl Pts',(92.8019633485471,1.28205441484255,1.79432370752333));
#10020=CARTESIAN_POINT('Ctrl Pts',(92.8060218752458,1.21946920537885,1.8358951106021));
#10021=CARTESIAN_POINT('Ctrl Pts',(92.8100845522973,1.1568199946859,1.87750902565647));
#10022=CARTESIAN_POINT('Ctrl Pts',(92.8141472293487,1.09206573244855,1.91589428290774));
#10023=CARTESIAN_POINT('Ctrl Pts',(92.8182099064002,1.02557726386979,1.9508478351305));
#10024=CARTESIAN_POINT('Ctrl Pts',(92.8222747054438,0.959054067449693,1.98581964407419));
#10025=CARTESIAN_POINT('Ctrl Pts',(92.8263395044873,0.890795294716255,2.01735597810705));
#10026=CARTESIAN_POINT('Ctrl Pts',(92.8304043035309,0.821193184476299,2.04530138458118));
#10027=CARTESIAN_POINT('Ctrl Pts',(92.8344763638389,0.751466738611704,2.07329671209301));
#10028=CARTESIAN_POINT('Ctrl Pts',(92.8385484241469,0.680392614288185,2.09768814386498));
#10029=CARTESIAN_POINT('Ctrl Pts',(92.8426204844549,0.608379235982138,2.11836982258193));
#10030=CARTESIAN_POINT('Ctrl Pts',(92.8457586346647,0.552881826526517,2.13430824428888));
#10031=CARTESIAN_POINT('Ctrl Pts',(92.8488967848745,0.496826933752397,2.14804443234602));
#10032=CARTESIAN_POINT('Ctrl Pts',(92.8520349350843,0.440404527712738,2.15955084496062));
#10033=CARTESIAN_POINT('Ctrl Pts',(92.8578492539753,0.335865917584354,2.1808697582563));
#10034=CARTESIAN_POINT('Ctrl Pts',(92.8636635728662,0.229731969372485,2.19460365402509));
#10035=CARTESIAN_POINT('Ctrl Pts',(92.8694778917572,0.122912597202681,2.20057003829664));
#10036=CARTESIAN_POINT('Ctrl Pts',(92.8716680634389,0.082675250682759,2.20281749085632));
#10037=CARTESIAN_POINT('Ctrl Pts',(92.8738582351207,0.0423408978578493,
2.20396323092196));
#10038=CARTESIAN_POINT('Ctrl Pts',(92.8760484068025,0.00195929810404175,
2.20399912911756));
#10039=CARTESIAN_POINT('',(93.6260484067633,4.74792226950262E-5,2.20399999948859));
#10040=CARTESIAN_POINT('Ctrl Pts',(92.8760484068423,0.00195929737048818,
2.20399912911821));
#10041=CARTESIAN_POINT('Ctrl Pts',(92.8800549703073,-0.0719122824601498,
2.20406479901354));
#10042=CARTESIAN_POINT('Ctrl Pts',(92.8840615337723,-0.145903667991656,
2.20041230851384));
#10043=CARTESIAN_POINT('Ctrl Pts',(92.8880680972373,-0.219604015837993,
2.19303216488674));
#10044=CARTESIAN_POINT('Ctrl Pts',(92.892071309022,-0.293242709849697,2.18565819509963));
#10045=CARTESIAN_POINT('Ctrl Pts',(92.8960745208068,-0.3665903610426,2.17456280216026));
#10046=CARTESIAN_POINT('Ctrl Pts',(92.9000777325915,-0.439237413510549,
2.15978853005857));
#10047=CARTESIAN_POINT('Ctrl Pts',(92.9040789764028,-0.511848752786769,
2.14502152096886));
#10048=CARTESIAN_POINT('Ctrl Pts',(92.9080802202141,-0.583759694539525,
2.1265793172489));
#10049=CARTESIAN_POINT('Ctrl Pts',(92.9120814640254,-0.654568895058323,
2.10455590603389));
#10050=CARTESIAN_POINT('Ctrl Pts',(92.9160821208197,-0.725367707256604,
2.08253572584328));
#10051=CARTESIAN_POINT('Ctrl Pts',(92.920082777614,-0.795064629188487,2.05693552828468));
#10052=CARTESIAN_POINT('Ctrl Pts',(92.9240834344083,-0.863273309956541,
2.0278992066463));
#10053=CARTESIAN_POINT('Ctrl Pts',(92.9280876445556,-0.931542573156908,
1.99883709516752));
#10054=CARTESIAN_POINT('Ctrl Pts',(92.9320918547029,-0.998320500086283,
1.96633295551533));
#10055=CARTESIAN_POINT('Ctrl Pts',(92.9360960648502,-1.06324149190924,1.93057854797017));
#10056=CARTESIAN_POINT('Ctrl Pts',(92.9401019558659,-1.12818973595942,1.89480913160874));
#10057=CARTESIAN_POINT('Ctrl Pts',(92.9441078468817,-1.19127907374594,1.85578699064998));
#10058=CARTESIAN_POINT('Ctrl Pts',(92.9481137378974,-1.25217171549734,1.81374805166221));
#10059=CARTESIAN_POINT('Ctrl Pts',(92.9521268553409,-1.31317420454101,1.77163327652273));
#10060=CARTESIAN_POINT('Ctrl Pts',(92.9561399727845,-1.37197169089296,1.72649113356451));
#10061=CARTESIAN_POINT('Ctrl Pts',(92.960153090228,-1.42825884302409,1.67859842646283));
#10062=CARTESIAN_POINT('Ctrl Pts',(92.9638306105198,-1.47983897917582,1.63471074944508));
#10063=CARTESIAN_POINT('Ctrl Pts',(92.9675081308117,-1.52931129181564,1.58851397528272));
#10064=CARTESIAN_POINT('Ctrl Pts',(92.9711856511035,-1.5764697644302,1.54024643542435));
#10065=CARTESIAN_POINT('Ctrl Pts',(92.9752587160244,-1.62870048113314,1.48678736305582));
#10066=CARTESIAN_POINT('Ctrl Pts',(92.9793317809454,-1.67830959326401,1.43056542275226));
#10067=CARTESIAN_POINT('Ctrl Pts',(92.9834048458663,-1.72499095324703,1.3718681464397));
#10068=CARTESIAN_POINT('Ctrl Pts',(92.987471926656,-1.77160372915663,1.31325710793833));
#10069=CARTESIAN_POINT('Ctrl Pts',(92.9915390074458,-1.81529699831034,1.25217832445775));
#10070=CARTESIAN_POINT('Ctrl Pts',(92.9956060882355,-1.85580183704518,1.1889556516623));
#10071=CARTESIAN_POINT('Ctrl Pts',(92.9996684105887,-1.89625928559648,1.12580694864828));
#10072=CARTESIAN_POINT('Ctrl Pts',(93.0037307329418,-1.93353545896034,1.06051973979805));
#10073=CARTESIAN_POINT('Ctrl Pts',(93.007793055295,-1.96740309055949,0.99344908236757));
#10074=CARTESIAN_POINT('Ctrl Pts',(93.0118527994184,-2.0012492274252,0.926420992599341));
#10075=CARTESIAN_POINT('Ctrl Pts',(93.0159125435418,-2.0316909006833,0.857612125508566));
#10076=CARTESIAN_POINT('Ctrl Pts',(93.0199722876652,-2.05854608239204,0.78740334433402));
#10077=CARTESIAN_POINT('Ctrl Pts',(93.0240307671041,-2.0853928982212,0.717216434477091));
#10078=CARTESIAN_POINT('Ctrl Pts',(93.0280892465431,-2.10865527030138,0.645630922051442));
#10079=CARTESIAN_POINT('Ctrl Pts',(93.0321477259821,-2.12819939080647,0.57304742645872));
#10080=CARTESIAN_POINT('Ctrl Pts',(93.0362062525982,-2.14774373849916,0.500463087130436));
#10081=CARTESIAN_POINT('Ctrl Pts',(93.0402647792143,-2.16356962638733,0.426881203107006));
#10082=CARTESIAN_POINT('Ctrl Pts',(93.0443233058304,-2.17559361893673,0.352715757008075));
#10083=CARTESIAN_POINT('Ctrl Pts',(93.0483859827991,-2.1876299075268,0.278474467437261));
#10084=CARTESIAN_POINT('Ctrl Pts',(93.0524486597678,-2.19585646025411,0.203648896438431));
#10085=CARTESIAN_POINT('Ctrl Pts',(93.0565113367365,-2.20024145044579,0.12866063788201));
#10086=CARTESIAN_POINT('Ctrl Pts',(93.060576135697,-2.20462873097793,0.0536332119307196));
#10087=CARTESIAN_POINT('Ctrl Pts',(93.0646409346575,-2.20517044978059,-0.0215565929029333));
#10088=CARTESIAN_POINT('Ctrl Pts',(93.0687057336181,-2.20188696162339,-0.0964873475276276));
#10089=CARTESIAN_POINT('Ctrl Pts',(93.0727777938436,-2.19859760791717,-0.171551956758485));
#10090=CARTESIAN_POINT('Ctrl Pts',(93.0768498540691,-2.19146944369823,-0.246356115437402));
#10091=CARTESIAN_POINT('Ctrl Pts',(93.0809219142946,-2.18057467730157,-0.320484128641563));
#10092=CARTESIAN_POINT('Ctrl Pts',(93.0840600652373,-2.17217857814179,-0.377611204773327));
#10093=CARTESIAN_POINT('Ctrl Pts',(93.0871982161799,-2.16154653352215,-0.434336816769531));
#10094=CARTESIAN_POINT('Ctrl Pts',(93.0903363671226,-2.14873188981487,-0.49047656997314));
#10095=CARTESIAN_POINT('Ctrl Pts',(93.0944094320672,-2.13209952348991,-0.56334140820073));
#10096=CARTESIAN_POINT('Ctrl Pts',(93.0984824970118,-2.11172454344625,-0.635499781504664));
#10097=CARTESIAN_POINT('Ctrl Pts',(93.1025555619564,-2.08768274156705,-0.706538583916761));
#10098=CARTESIAN_POINT('Ctrl Pts',(93.1066226427702,-2.06367626180753,-0.777473016402938));
#10099=CARTESIAN_POINT('Ctrl Pts',(93.1106897235839,-2.03601380795103,-0.847290695225555));
#10100=CARTESIAN_POINT('Ctrl Pts',(93.1147568043977,-2.00482187045235,-0.915590119953207));
#10101=CARTESIAN_POINT('Ctrl Pts',(93.1188191267755,-1.9736664271486,-0.983809635168375));
#10102=CARTESIAN_POINT('Ctrl Pts',(93.1228814491532,-1.93898990183575,-1.05051399333959));
#10103=CARTESIAN_POINT('Ctrl Pts',(93.1269437715309,-1.9009675803897,-1.11531980091243));
#10104=CARTESIAN_POINT('Ctrl Pts',(93.1310035156792,-1.86296939052679,-1.1800844782577));
#10105=CARTESIAN_POINT('Ctrl Pts',(93.1350632598274,-1.82162985933606,-1.24295258532953));
#10106=CARTESIAN_POINT('Ctrl Pts',(93.1391230039756,-1.77717047369368,-1.30356476917389));
#10107=CARTESIAN_POINT('Ctrl Pts',(93.1431814834397,-1.73272493795903,-1.36415807121993));
#10108=CARTESIAN_POINT('Ctrl Pts',(93.1472399629038,-1.68516175963341,-1.42249646059683));
#10109=CARTESIAN_POINT('Ctrl Pts',(93.1512984423678,-1.63474515718172,-1.47825040878428));
#10110=CARTESIAN_POINT('Ctrl Pts',(93.1553569690093,-1.58432796866732,-1.5340050050779));
#10111=CARTESIAN_POINT('Ctrl Pts',(93.1594154956507,-1.53105761173668,-1.58717474759307));
#10112=CARTESIAN_POINT('Ctrl Pts',(93.1634740222921,-1.47523682930359,-1.63746520496355));
#10113=CARTESIAN_POINT('Ctrl Pts',(93.1675366992863,-1.41935896311644,-1.68780709063678));
#10114=CARTESIAN_POINT('Ctrl Pts',(93.1715993762805,-1.36092581865817,-1.73526349100998));
#10115=CARTESIAN_POINT('Ctrl Pts',(93.1756620532747,-1.30027449879505,-1.77957922773427));
#10116=CARTESIAN_POINT('Ctrl Pts',(93.1797268522608,-1.23959149991492,-1.82391811117623));
#10117=CARTESIAN_POINT('Ctrl Pts',(93.183791651247,-1.17668841822423,-1.86511280242322));
#10118=CARTESIAN_POINT('Ctrl Pts',(93.1878564502331,-1.11193049106998,-1.90295207060737));
#10119=CARTESIAN_POINT('Ctrl Pts',(93.1919285104841,-1.04705688182033,-1.94085893400379));
#10120=CARTESIAN_POINT('Ctrl Pts',(93.1960005707352,-0.980322233403132,
-1.97539818189542));
#10121=CARTESIAN_POINT('Ctrl Pts',(93.2000726309862,-0.912115058956017,
-2.0064052729261));
#10122=CARTESIAN_POINT('Ctrl Pts',(93.2032107817047,-0.859550907076969,
-2.03030102077779));
#10123=CARTESIAN_POINT('Ctrl Pts',(93.2063489324232,-0.806112702462154,
-2.05209994820842));
#10124=CARTESIAN_POINT('Ctrl Pts',(93.2094870831417,-0.751984331871373,
-2.07174698373618));
#10125=CARTESIAN_POINT('Ctrl Pts',(93.2135601480768,-0.681730099992325,
-2.09724724126542));
#10126=CARTESIAN_POINT('Ctrl Pts',(93.2176332130119,-0.610041822848098,
-2.11921907646067));
#10127=CARTESIAN_POINT('Ctrl Pts',(93.221706277947,-0.537307779208416,-2.13750236266586));
#10128=CARTESIAN_POINT('Ctrl Pts',(93.2257733587512,-0.464680596138525,
-2.15575878713913));
#10129=CARTESIAN_POINT('Ctrl Pts',(93.2298404395554,-0.391011156236629,
-2.17033730651605));
#10130=CARTESIAN_POINT('Ctrl Pts',(93.2339075203595,-0.316705453413108,
-2.1811266941144));
#10131=CARTESIAN_POINT('Ctrl Pts',(93.2379698427276,-0.242486687378207,
-2.19190345825757));
#10132=CARTESIAN_POINT('Ctrl Pts',(93.2420321650956,-0.167633607545572,
-2.19889983019213));
#10133=CARTESIAN_POINT('Ctrl Pts',(93.2460944874636,-0.0925634274613625,
-2.20205540618228));
#10134=CARTESIAN_POINT('Ctrl Pts',(93.250154231602,-0.0175408920837323,
-2.20520897942658));
#10135=CARTESIAN_POINT('Ctrl Pts',(93.2542139757405,0.0576979942920653,
-2.20452657394543));
#10136=CARTESIAN_POINT('Ctrl Pts',(93.2582737198789,0.132731191454727,-2.19999964336702));
#10137=CARTESIAN_POINT('Ctrl Pts',(93.2623321993331,0.207741014410062,-2.19547412300992));
#10138=CARTESIAN_POINT('Ctrl Pts',(93.2663906787874,0.282544799089149,-2.18710648415298));
#10139=CARTESIAN_POINT('Ctrl Pts',(93.2704491582416,0.356722419692342,-2.17494025556769));
#10140=CARTESIAN_POINT('Ctrl Pts',(93.2745076848732,0.43090090256517,-2.1627738855574));
#10141=CARTESIAN_POINT('Ctrl Pts',(93.2785662115047,0.504452736034628,-2.14680891719227));
#10142=CARTESIAN_POINT('Ctrl Pts',(93.2826247381363,0.576966419918423,-2.12714027517851));
#10143=CARTESIAN_POINT('Ctrl Pts',(93.2866874151206,0.649554258142763,-2.10745151951034));
#10144=CARTESIAN_POINT('Ctrl Pts',(93.2907500921049,0.721101364916498,-2.08405165209815));
#10145=CARTESIAN_POINT('Ctrl Pts',(93.2948127690892,0.791210615063416,-2.05708574507991));
#10146=CARTESIAN_POINT('Ctrl Pts',(93.2988775680654,0.861356484234057,-2.03010575339828));
#10147=CARTESIAN_POINT('Ctrl Pts',(93.3029423670417,0.930062564526948,-1.99955620710848));
#10148=CARTESIAN_POINT('Ctrl Pts',(93.307007166018,0.996953424529923,-1.96562963686399));
#10149=CARTESIAN_POINT('Ctrl Pts',(93.3110792262592,1.06396377685304,-1.93164246096138));
#10150=CARTESIAN_POINT('Ctrl Pts',(93.3151512865005,1.1291520170853,-1.89426644921628));
#10151=CARTESIAN_POINT('Ctrl Pts',(93.3192233467418,1.19216934477753,-1.85373899278532));
#10152=CARTESIAN_POINT('Ctrl Pts',(93.3223614975481,1.24073392044573,-1.82250633350637));
#10153=CARTESIAN_POINT('Ctrl Pts',(93.3254996483545,1.2880097103385,-1.78940293750926));
#10154=CARTESIAN_POINT('Ctrl Pts',(93.3286377991608,1.33385079356041,-1.75455352170239));
#10155=CARTESIAN_POINT('Ctrl Pts',(93.3327108640952,1.39334879736683,-1.70932180969656));
#10156=CARTESIAN_POINT('Ctrl Pts',(93.3367839290295,1.45065817780139,-1.66097301929738));
#10157=CARTESIAN_POINT('Ctrl Pts',(93.3408569939638,1.50543397192874,-1.60974673665234));
#10158=CARTESIAN_POINT('Ctrl Pts',(93.3449240747671,1.560129289675,-1.55859571546009));
#10159=CARTESIAN_POINT('Ctrl Pts',(93.3489911555705,1.61229806563741,-1.50457591895396));
#10160=CARTESIAN_POINT('Ctrl Pts',(93.3530582363738,1.6616268385985,-1.44796831776429));
#10161=CARTESIAN_POINT('Ctrl Pts',(93.3571205587409,1.71089789748109,-1.3914269467957));
#10162=CARTESIAN_POINT('Ctrl Pts',(93.361182881108,1.75733524284504,-1.33230414464942));
#10163=CARTESIAN_POINT('Ctrl Pts',(93.3652452034752,1.80066205083603,-1.27091784891038));
#10164=CARTESIAN_POINT('Ctrl Pts',(93.3693049476127,1.84396136065031,-1.20957051314292));
#10165=CARTESIAN_POINT('Ctrl Pts',(93.3733646917502,1.88415377597543,-1.14596292359402));
#10166=CARTESIAN_POINT('Ctrl Pts',(93.3774244358877,1.92100344358486,-1.08044517201712));
#10167=CARTESIAN_POINT('Ctrl Pts',(93.3814829153409,1.9578416318513,-1.0149478304138));
#10168=CARTESIAN_POINT('Ctrl Pts',(93.3855413947942,1.99133890600378,-0.947541924111951));
#10169=CARTESIAN_POINT('Ctrl Pts',(93.3895998742474,2.02130421893966,-0.878604151194797));
#10170=CARTESIAN_POINT('Ctrl Pts',(93.393658400878,2.05126988020382,-0.809665576918541));
#10171=CARTESIAN_POINT('Ctrl Pts',(93.3977169275086,2.07770331004053,-0.739195539267929));
#10172=CARTESIAN_POINT('Ctrl Pts',(93.4017754541391,2.10046133286916,-0.667591333917327));
#10173=CARTESIAN_POINT('Ctrl Pts',(93.4058381311224,2.12324262863151,-0.595913904282804));
#10174=CARTESIAN_POINT('Ctrl Pts',(93.4099008081056,2.14234086680234,-0.52310044687806));
#10175=CARTESIAN_POINT('Ctrl Pts',(93.4139634850889,2.15766280910038,-0.449563346176113));
#10176=CARTESIAN_POINT('Ctrl Pts',(93.4180282840641,2.17299275425912,-0.375987836037407));
#10177=CARTESIAN_POINT('Ctrl Pts',(93.4220930830392,2.18454240227297,-0.301688402146922));
#10178=CARTESIAN_POINT('Ctrl Pts',(93.4261578820144,2.1922701575948,-0.227084909492602));
#10179=CARTESIAN_POINT('Ctrl Pts',(93.4302299422546,2.20001171760397,-0.152348146846223));
#10180=CARTESIAN_POINT('Ctrl Pts',(93.4343020024947,2.20391772297867,-0.0773067180315107));
#10181=CARTESIAN_POINT('Ctrl Pts',(93.4383740627349,2.20399871236733,-0.00238241120780133));
#10182=CARTESIAN_POINT('Ctrl Pts',(93.4415122135499,2.20406112718956,0.0553583295131656));
#10183=CARTESIAN_POINT('Ctrl Pts',(93.444650364365,2.2018529080311,0.113029456811266));
#10184=CARTESIAN_POINT('Ctrl Pts',(93.44778851518,2.19739981579467,0.170440750836054));
#10185=CARTESIAN_POINT('Ctrl Pts',(93.4518615801172,2.19162006366708,0.244955948628872));
#10186=CARTESIAN_POINT('Ctrl Pts',(93.4559346450543,2.18203458412387,0.319320518212626));
#10187=CARTESIAN_POINT('Ctrl Pts',(93.4600077099914,2.16865783993518,0.393114707544327));
#10188=CARTESIAN_POINT('Ctrl Pts',(93.4640747907976,2.1553007488062,0.46680047874468));
#10189=CARTESIAN_POINT('Ctrl Pts',(93.4681418716038,2.13816353642985,0.539917067561367));
#10190=CARTESIAN_POINT('Ctrl Pts',(93.4722089524101,2.11731251727188,0.612048776000599));
#10191=CARTESIAN_POINT('Ctrl Pts',(93.4762712747801,2.09648589355834,0.684096091198791));
#10192=CARTESIAN_POINT('Ctrl Pts',(93.4803335971501,2.07195422772864,0.755160358996972));
#10193=CARTESIAN_POINT('Ctrl Pts',(93.4843959195202,2.04383475563522,0.824836645438059));
#10194=CARTESIAN_POINT('Ctrl Pts',(93.4884556636607,2.01573313009541,0.894468710509103));
#10195=CARTESIAN_POINT('Ctrl Pts',(93.4925154078012,1.98404839512368,0.962714100649501));
#10196=CARTESIAN_POINT('Ctrl Pts',(93.4965751519417,1.94894701069206,1.02918489568906));
#10197=CARTESIAN_POINT('Ctrl Pts',(93.5006336313979,1.91385656098102,1.09563498386526));
#10198=CARTESIAN_POINT('Ctrl Pts',(93.5046921108542,1.87535179783926,1.16031115260634));
#10199=CARTESIAN_POINT('Ctrl Pts',(93.5087505903104,1.83364582058261,1.22284872517411));
#10200=CARTESIAN_POINT('Ctrl Pts',(93.512809116944,1.79193935851936,1.28538702470308));
#10201=CARTESIAN_POINT('Ctrl Pts',(93.5168676435776,1.74703187485705,1.34578628246384));
#10202=CARTESIAN_POINT('Ctrl Pts',(93.5209261702112,1.69917971884093,1.40371089725757));
#10203=CARTESIAN_POINT('Ctrl Pts',(93.5249888471975,1.65127862799127,1.46169474723773));
#10204=CARTESIAN_POINT('Ctrl Pts',(93.5290515241838,1.60042715616635,1.51719853180398));
#10205=CARTESIAN_POINT('Ctrl Pts',(93.5331142011701,1.54692139171317,1.56992044634759));
#10206=CARTESIAN_POINT('Ctrl Pts',(93.5371790001484,1.49338768046484,1.62266989827076));
#10207=CARTESIAN_POINT('Ctrl Pts',(93.5412437991266,1.43719727289644,1.67263426908128));
#10208=CARTESIAN_POINT('Ctrl Pts',(93.5453085981049,1.37868052577792,1.71955110649283));
#10209=CARTESIAN_POINT('Ctrl Pts',(93.5493806583481,1.32005924566588,1.76655175508157));
#10210=CARTESIAN_POINT('Ctrl Pts',(93.5534527185913,1.25910371316289,1.81049371659205));
#10211=CARTESIAN_POINT('Ctrl Pts',(93.5575247788346,1.19617414883073,1.85115731521367));
#10212=CARTESIAN_POINT('Ctrl Pts',(93.5606629296228,1.14767720867898,1.88249489286315));
#10213=CARTESIAN_POINT('Ctrl Pts',(93.563801080411,1.09800850212365,1.91188629785332));
#10214=CARTESIAN_POINT('Ctrl Pts',(93.5669392311991,1.04734186562866,1.93925011705594));
#10215=CARTESIAN_POINT('Ctrl Pts',(93.5712291614867,0.97807931161546,1.97665713944072));
#10216=CARTESIAN_POINT('Ctrl Pts',(93.5755190917743,0.906707522894725,2.01040537985972));
#10217=CARTESIAN_POINT('Ctrl Pts',(93.5798090220618,0.833627277572188,2.04026507152565));
#10218=CARTESIAN_POINT('Ctrl Pts',(93.5840864142973,0.760760621716913,2.07003749315565));
#10219=CARTESIAN_POINT('Ctrl Pts',(93.5883638065327,0.686195825607445,2.09594385041639));
#10220=CARTESIAN_POINT('Ctrl Pts',(93.5926411987682,0.610356510638483,2.11780096560588));
#10221=CARTESIAN_POINT('Ctrl Pts',(93.5969110194947,0.534651440558738,2.13961939102071));
#10222=CARTESIAN_POINT('Ctrl Pts',(93.6011808402213,0.457676723409933,2.15740271911496));
#10223=CARTESIAN_POINT('Ctrl Pts',(93.6054506609479,0.379874733097137,2.17101616464604));
#10224=CARTESIAN_POINT('Ctrl Pts',(93.6097108188649,0.302248812427545,2.18459880229562));
#10225=CARTESIAN_POINT('Ctrl Pts',(93.613970976782,0.223799742236276,2.19403028120832));
#10226=CARTESIAN_POINT('Ctrl Pts',(93.618231134699,0.144982223500534,2.19922626277262));
#10227=CARTESIAN_POINT('Ctrl Pts',(93.6208368920538,0.0967729004828302,
2.20240442363896));
#10228=CARTESIAN_POINT('Ctrl Pts',(93.6234426494085,0.0484260077747917,
2.20399895730396));
#10229=CARTESIAN_POINT('Ctrl Pts',(93.6260484067633,4.74792226957855E-5,
2.2039999994886));
#10230=CARTESIAN_POINT('',(94.3760484067719,-0.00198161751639934,2.20399910916316));
#10231=CARTESIAN_POINT('Ctrl Pts',(93.6260484068025,4.74784943464956E-5,
2.20399999948861));
#10232=CARTESIAN_POINT('Ctrl Pts',(93.6302924706585,-0.0787478721400754,
2.20400169689542));
#10233=CARTESIAN_POINT('Ctrl Pts',(93.6345365345146,-0.157464660372779,
2.19977356426505));
#10234=CARTESIAN_POINT('Ctrl Pts',(93.6387805983706,-0.235645064551175,
2.1913665607453));
#10235=CARTESIAN_POINT('Ctrl Pts',(93.6430360559872,-0.314035354545841,
2.18293698749321));
#10236=CARTESIAN_POINT('Ctrl Pts',(93.6472915136038,-0.391885973482654,
2.17030616852904));
#10237=CARTESIAN_POINT('Ctrl Pts',(93.6515469712204,-0.468746913744802,
2.15357663686592));
#10238=CARTESIAN_POINT('Ctrl Pts',(93.6558083437779,-0.545714688092428,
2.13682385172438));
#10239=CARTESIAN_POINT('Ctrl Pts',(93.6600697163354,-0.621689645794342,
2.11596110459831));
#10240=CARTESIAN_POINT('Ctrl Pts',(93.664331088893,-0.696237353990324,2.09114072862363));
#10241=CARTESIAN_POINT('Ctrl Pts',(93.6686040125675,-0.770987135410994,
2.06625307313717));
#10242=CARTESIAN_POINT('Ctrl Pts',(93.6728769362419,-0.844301550522626,
2.03738649373384));
#10243=CARTESIAN_POINT('Ctrl Pts',(93.6771498599164,-0.915765840088244,
2.00474161081359));
#10244=CARTESIAN_POINT('Ctrl Pts',(93.6801298890171,-0.96560657649917,1.98197436559667));
#10245=CARTESIAN_POINT('Ctrl Pts',(93.6831099181177,-1.01454790143108,1.95737035493228));
#10246=CARTESIAN_POINT('Ctrl Pts',(93.6860899472184,-1.06245716940618,1.93101029597913));
#10247=CARTESIAN_POINT('Ctrl Pts',(93.6901630121542,-1.12793893246917,1.89498171095476));
#10248=CARTESIAN_POINT('Ctrl Pts',(93.69423607709,-1.19171226772072,1.85554908062932));
#10249=CARTESIAN_POINT('Ctrl Pts',(93.6983091420258,-1.25340083861911,1.8128988768679));
#10250=CARTESIAN_POINT('Ctrl Pts',(93.7023762228307,-1.31499877691252,1.77031133461759));
#10251=CARTESIAN_POINT('Ctrl Pts',(93.7064433036356,-1.374517642539,1.72451587371866));
#10252=CARTESIAN_POINT('Ctrl Pts',(93.7105103844404,-1.43160619890503,1.67574451849221));
#10253=CARTESIAN_POINT('Ctrl Pts',(93.7145727068091,-1.48862796233871,1.62703022517165));
#10254=CARTESIAN_POINT('Ctrl Pts',(93.7186350291778,-1.54322470456571,1.57534726356366));
#10255=CARTESIAN_POINT('Ctrl Pts',(93.7226973515465,-1.59507601626904,1.52096959283323));
#10256=CARTESIAN_POINT('Ctrl Pts',(93.7267570956856,-1.64689441955874,1.46662643391788));
#10257=CARTESIAN_POINT('Ctrl Pts',(93.7308168398247,-1.69597052134901,1.40959230435394));
#10258=CARTESIAN_POINT('Ctrl Pts',(93.7348765839638,-1.74201973109914,1.35017897201122));
#10259=CARTESIAN_POINT('Ctrl Pts',(93.7389350634187,-1.7880545956816,1.29078414800381));
#10260=CARTESIAN_POINT('Ctrl Pts',(93.7429935428735,-1.83106414807162,1.22901196990301));
#10261=CARTESIAN_POINT('Ctrl Pts',(93.7470520223284,-1.87080422327517,1.16520708810743));
#10262=CARTESIAN_POINT('Ctrl Pts',(93.7511105489606,-1.91054476043274,1.10140146461919));
#10263=CARTESIAN_POINT('Ctrl Pts',(93.7551690755927,-1.94701549404096,1.03556349674723));
#10264=CARTESIAN_POINT('Ctrl Pts',(93.7592276022249,-1.98001659714391,0.968065222510682));
#10265=CARTESIAN_POINT('Ctrl Pts',(93.7632902792098,-2.0130514480154,0.900497922819763));
#10266=CARTESIAN_POINT('Ctrl Pts',(93.7673529561947,-2.04260937278205,0.831267356102898));
#10267=CARTESIAN_POINT('Ctrl Pts',(93.7714156331796,-2.06853773294696,0.76076780122101));
#10268=CARTESIAN_POINT('Ctrl Pts',(93.7754804321565,-2.09447963585023,0.69023142345406));
#10269=CARTESIAN_POINT('Ctrl Pts',(93.7795452311333,-2.11678805711947,0.618425193987838));
#10270=CARTESIAN_POINT('Ctrl Pts',(93.7836100301101,-2.13536034821463,0.545758356118066));
#10271=CARTESIAN_POINT('Ctrl Pts',(93.7876820903519,-2.15396581643057,0.47296170785255));
#10272=CARTESIAN_POINT('Ctrl Pts',(93.7917541505937,-2.16882172886429,0.399301849134778));
#10273=CARTESIAN_POINT('Ctrl Pts',(93.7958262108356,-2.17987672713035,0.325197562284023));
#10274=CARTESIAN_POINT('Ctrl Pts',(93.7989643616362,-2.18839630925815,0.268088773783823));
#10275=CARTESIAN_POINT('Ctrl Pts',(93.8021025124368,-2.19465955223917,0.210716246280975));
#10276=CARTESIAN_POINT('Ctrl Pts',(93.8052406632374,-2.19866407578353,0.153271921299827));
#10277=CARTESIAN_POINT('Ctrl Pts',(93.8093137281735,-2.20386162219569,0.0787138516827568));
#10278=CARTESIAN_POINT('Ctrl Pts',(93.8133867931097,-2.20527242698567,0.00374732412319403));
#10279=CARTESIAN_POINT('Ctrl Pts',(93.8174598580458,-2.20284931181229,-0.0712103184104735));
#10280=CARTESIAN_POINT('Ctrl Pts',(93.821526938851,-2.20042975667016,-0.146057833471603));
#10281=CARTESIAN_POINT('Ctrl Pts',(93.8255940196562,-2.19418748022996,-0.220896016174146));
#10282=CARTESIAN_POINT('Ctrl Pts',(93.8296611004614,-2.18412719039319,-0.295303938655015));
#10283=CARTESIAN_POINT('Ctrl Pts',(93.8337234228304,-2.17407867097592,-0.369624804751169));
#10284=CARTESIAN_POINT('Ctrl Pts',(93.8377857451995,-2.16022107678299,-0.443515939987352));
#10285=CARTESIAN_POINT('Ctrl Pts',(93.8418480675685,-2.14261106456059,-0.516559605488601));
#10286=CARTESIAN_POINT('Ctrl Pts',(93.845907811708,-2.12501222886481,-0.589556912448955));
#10287=CARTESIAN_POINT('Ctrl Pts',(93.8499675558474,-2.10366581267472,-0.661707354019261));
#10288=CARTESIAN_POINT('Ctrl Pts',(93.8540272999869,-2.07867965808225,-0.732602811266139));
#10289=CARTESIAN_POINT('Ctrl Pts',(93.8580857794421,-2.05370128713207,-0.803476183286705));
#10290=CARTESIAN_POINT('Ctrl Pts',(93.8621442588973,-2.02508558758278,-0.873094897180993));
#10291=CARTESIAN_POINT('Ctrl Pts',(93.8662027383525,-1.99298994249238,-0.941066995024375));
#10292=CARTESIAN_POINT('Ctrl Pts',(93.8702612649851,-1.96089392430978,-1.00903988300173));
#10293=CARTESIAN_POINT('Ctrl Pts',(93.8743197916176,-1.92531808575484,-1.07536568593995));
#10294=CARTESIAN_POINT('Ctrl Pts',(93.8783783182502,-1.88646685228122,-1.13967487260368));
#10295=CARTESIAN_POINT('Ctrl Pts',(93.8824409952354,-1.84757588854667,-1.20404982347969));
#10296=CARTESIAN_POINT('Ctrl Pts',(93.8865036722207,-1.80540308856911,-1.26640363031909));
#10297=CARTESIAN_POINT('Ctrl Pts',(93.890566349206,-1.76019713877674,-1.32639437296838));
#10298=CARTESIAN_POINT('Ctrl Pts',(93.8946311481832,-1.71496757729636,-1.38641644960591));
#10299=CARTESIAN_POINT('Ctrl Pts',(93.8986959471604,-1.66670201787713,-1.44407263769095));
#10300=CARTESIAN_POINT('Ctrl Pts',(93.9027607461376,-1.61568881005288,-1.49905492530124));
#10301=CARTESIAN_POINT('Ctrl Pts',(93.9068328063798,-1.56458447338786,-1.55413543202667));
#10302=CARTESIAN_POINT('Ctrl Pts',(93.9109048666219,-1.51072302704085,-1.60653216397486));
#10303=CARTESIAN_POINT('Ctrl Pts',(93.9149769268641,-1.45442862809842,-1.65597504986269));
#10304=CARTESIAN_POINT('Ctrl Pts',(93.9181150776616,-1.41104510663045,-1.69407842322932));
#10305=CARTESIAN_POINT('Ctrl Pts',(93.9212532284591,-1.36621738319208,-1.7304282558195));
#10306=CARTESIAN_POINT('Ctrl Pts',(93.9243913792565,-1.32010549383252,-1.76491854915551));
#10307=CARTESIAN_POINT('Ctrl Pts',(93.9284644441925,-1.26025600545494,-1.809684149499));
#10308=CARTESIAN_POINT('Ctrl Pts',(93.9325375091285,-1.19801147619516,-1.8514883263379));
#10309=CARTESIAN_POINT('Ctrl Pts',(93.9366105740644,-1.13369711820735,-1.89006530156192));
#10310=CARTESIAN_POINT('Ctrl Pts',(93.9406776548695,-1.06947725062046,-1.9285855996462));
#10311=CARTESIAN_POINT('Ctrl Pts',(93.9447447356745,-1.00319399795282,-1.9638878661549));
#10312=CARTESIAN_POINT('Ctrl Pts',(93.9488118164795,-0.935203698473259,
-1.9957479906947));
#10313=CARTESIAN_POINT('Ctrl Pts',(93.9528741388484,-0.867292946835827,
-2.02757083926754));
#10314=CARTESIAN_POINT('Ctrl Pts',(93.9569364612172,-0.797679546589344,
-2.05595934554963));
#10315=CARTESIAN_POINT('Ctrl Pts',(93.960998783586,-0.726745302627086,-2.08073478970999));
#10316=CARTESIAN_POINT('Ctrl Pts',(93.9650585277253,-0.655856078421628,
-2.10549450966708));
#10317=CARTESIAN_POINT('Ctrl Pts',(93.9691182718646,-0.583648123627884,
-2.12664556086921));
#10318=CARTESIAN_POINT('Ctrl Pts',(93.9731780160039,-0.51052289090503,-2.14405745675389));
#10319=CARTESIAN_POINT('Ctrl Pts',(93.9772364954589,-0.437420438024153,
-2.16146392851585));
#10320=CARTESIAN_POINT('Ctrl Pts',(93.9812949749139,-0.363401738728236,
-2.17513344712636));
#10321=CARTESIAN_POINT('Ctrl Pts',(93.9853534543689,-0.288881504754601,
-2.18498592128433));
#10322=CARTESIAN_POINT('Ctrl Pts',(93.9894119810013,-0.214360404529088,
-2.19483850997124));
#10323=CARTESIAN_POINT('Ctrl Pts',(93.9934705076336,-0.139338231626751,
-2.2008739053018));
#10324=CARTESIAN_POINT('Ctrl Pts',(93.997529034266,-0.0642363368181861,
-2.20306370607665));
#10325=CARTESIAN_POINT('Ctrl Pts',(94.001591711251,0.0109423591011084,-2.20525574619755));
#10326=CARTESIAN_POINT('Ctrl Pts',(94.0056543882361,0.0862004614105676,
-2.20359432463246));
#10327=CARTESIAN_POINT('Ctrl Pts',(94.0097170652212,0.161115844789395,-2.19810320152576));
#10328=CARTESIAN_POINT('Ctrl Pts',(94.0137818641982,0.236070357501068,-2.19260921033011));
#10329=CARTESIAN_POINT('Ctrl Pts',(94.0178466631752,0.310681320593962,-2.18328159346358));
#10330=CARTESIAN_POINT('Ctrl Pts',(94.0219114621522,0.384533618134413,-2.17019581985692));
#10331=CARTESIAN_POINT('Ctrl Pts',(94.0259835223942,0.458517843748993,-2.15708667012023));
#10332=CARTESIAN_POINT('Ctrl Pts',(94.0300555826361,0.531740230831165,-2.1402060613951));
#10333=CARTESIAN_POINT('Ctrl Pts',(94.0341276428781,0.603798151067578,-2.11968011567014));
#10334=CARTESIAN_POINT('Ctrl Pts',(94.0372657936773,0.659329898276897,-2.10386170701373));
#10335=CARTESIAN_POINT('Ctrl Pts',(94.0404039444765,0.714170302893095,-2.0858793505723));
#10336=CARTESIAN_POINT('Ctrl Pts',(94.0435420952757,0.768143562992485,-2.06581012356732));
#10337=CARTESIAN_POINT('Ctrl Pts',(94.0476151602117,0.838196472255843,-2.03976189643083));
#10338=CARTESIAN_POINT('Ctrl Pts',(94.0516882251476,0.907058004530739,-2.01009609125474));
#10339=CARTESIAN_POINT('Ctrl Pts',(94.0557612900836,0.974328568233429,-1.97694204293505));
#10340=CARTESIAN_POINT('Ctrl Pts',(94.0598283708887,1.04150029828942,-1.9438367044123));
#10341=CARTESIAN_POINT('Ctrl Pts',(94.0638954516937,1.10708527583775,-1.90725350710972));
#10342=CARTESIAN_POINT('Ctrl Pts',(94.0679625324988,1.17070206600156,-1.86737052366682));
#10343=CARTESIAN_POINT('Ctrl Pts',(94.0720248548676,1.23424442527713,-1.82753420284043));
#10344=CARTESIAN_POINT('Ctrl Pts',(94.0760871772365,1.2958227697159,-1.78440601856351));
#10345=CARTESIAN_POINT('Ctrl Pts',(94.0801494996053,1.35508001660587,-1.73821004156443));
#10346=CARTESIAN_POINT('Ctrl Pts',(94.0842092437446,1.41429965476574,-1.69204338371402));
#10347=CARTESIAN_POINT('Ctrl Pts',(94.0882689878839,1.47120074304027,-1.64281308962916));
#10348=CARTESIAN_POINT('Ctrl Pts',(94.0923287320232,1.5254560929374,-1.59078587764669));
#10349=CARTESIAN_POINT('Ctrl Pts',(94.0963872114782,1.5796945413047,-1.53877487308852));
#10350=CARTESIAN_POINT('Ctrl Pts',(94.1004456909333,1.63128854330689,-1.4839690107931));
#10351=CARTESIAN_POINT('Ctrl Pts',(94.1045041703883,1.6799460833365,-1.42667345846285));
#10352=CARTESIAN_POINT('Ctrl Pts',(94.1085626970207,1.72860418898035,-1.36937724010674));
#10353=CARTESIAN_POINT('Ctrl Pts',(94.1126212236531,1.77432545717723,-1.30959163934571));
#10354=CARTESIAN_POINT('Ctrl Pts',(94.1166797502854,1.81685772038635,-1.24765541070943));
#10355=CARTESIAN_POINT('Ctrl Pts',(94.1207424272705,1.859433478171,-1.18565584450841));
#10356=CARTESIAN_POINT('Ctrl Pts',(94.1248051042556,1.8988134477374,-1.1215016530489));
#10357=CARTESIAN_POINT('Ctrl Pts',(94.1288677812407,1.93478888318488,-1.05556050395238));
#10358=CARTESIAN_POINT('Ctrl Pts',(94.1329325802177,1.97078310909609,-0.989584912888582));
#10359=CARTESIAN_POINT('Ctrl Pts',(94.1369973791947,2.00336905259656,-0.921820936202544));
#10360=CARTESIAN_POINT('Ctrl Pts',(94.1410621781718,2.03238522655091,-0.852658367048386));
#10361=CARTESIAN_POINT('Ctrl Pts',(94.1451342384138,2.06145323434216,-0.783372247444925));
#10362=CARTESIAN_POINT('Ctrl Pts',(94.1492062986557,2.08693857293896,-0.712682994813434));
#10363=CARTESIAN_POINT('Ctrl Pts',(94.1532783588977,2.10872909485679,-0.64099735140206));
#10364=CARTESIAN_POINT('Ctrl Pts',(94.1564165096968,2.12552205461277,-0.585752500937799));
#10365=CARTESIAN_POINT('Ctrl Pts',(94.1595546604958,2.14012164517855,-0.529916248586732));
#10366=CARTESIAN_POINT('Ctrl Pts',(94.1626928112948,2.15249739642118,-0.473678116868447));
#10367=CARTESIAN_POINT('Ctrl Pts',(94.1667658762308,2.16856011668904,-0.400685588134812));
#10368=CARTESIAN_POINT('Ctrl Pts',(94.1708389411669,2.18093677105545,-0.326734326814922));
#10369=CARTESIAN_POINT('Ctrl Pts',(94.1749120061029,2.18951955782837,-0.252230263622469));
#10370=CARTESIAN_POINT('Ctrl Pts',(94.178979086908,2.19808973480484,-0.177835661505563));
#10371=CARTESIAN_POINT('Ctrl Pts',(94.1830461677131,2.20287705653575,-0.102890340399728));
#10372=CARTESIAN_POINT('Ctrl Pts',(94.1871132485181,2.20382452279676,-0.0278113775216291));
#10373=CARTESIAN_POINT('Ctrl Pts',(94.191175570887,2.2047708805335,0.047179743862388));
#10374=CARTESIAN_POINT('Ctrl Pts',(94.1952378932559,2.20188630254724,0.122303721344895));
#10375=CARTESIAN_POINT('Ctrl Pts',(94.1993002156248,2.19516564424378,0.197139022853949));
#10376=CARTESIAN_POINT('Ctrl Pts',(94.2033599597641,2.18844925133294,0.271926828726487));
#10377=CARTESIAN_POINT('Ctrl Pts',(94.2074197039035,2.17790165198512,0.346425847851594));
#10378=CARTESIAN_POINT('Ctrl Pts',(94.2114794480428,2.16356974397609,0.420216566726289));
#10379=CARTESIAN_POINT('Ctrl Pts',(94.2155379274979,2.14924230061747,0.493984298447898));
#10380=CARTESIAN_POINT('Ctrl Pts',(94.219596406953,2.13113298018927,0.567043699610763));
#10381=CARTESIAN_POINT('Ctrl Pts',(94.223654886408,2.10934005432727,0.638983986662144));
#10382=CARTESIAN_POINT('Ctrl Pts',(94.2277134130404,2.08754687513587,0.710925109975224));
#10383=CARTESIAN_POINT('Ctrl Pts',(94.2317719396729,2.06207014563213,0.781746636912583));
#10384=CARTESIAN_POINT('Ctrl Pts',(94.2358304663053,2.03305795748616,0.851053077958238));
#10385=CARTESIAN_POINT('Ctrl Pts',(94.2398931432904,2.00401610073764,0.92043039353579));
#10386=CARTESIAN_POINT('Ctrl Pts',(94.2439558202755,1.97143175027588,0.988289087819992));
#10387=CARTESIAN_POINT('Ctrl Pts',(94.2480184972606,1.93550082579324,1.05425450122524));
#10388=CARTESIAN_POINT('Ctrl Pts',(94.2520832962377,1.8995511340956,1.12025436927126));
#10389=CARTESIAN_POINT('Ctrl Pts',(94.2561480952148,1.86025163726231,1.18435857973248));
#10390=CARTESIAN_POINT('Ctrl Pts',(94.2602128941918,1.81784245713697,1.24622020567403));
#10391=CARTESIAN_POINT('Ctrl Pts',(94.2642849544339,1.77535751821137,1.30819233982512));
#10392=CARTESIAN_POINT('Ctrl Pts',(94.2683570146759,1.72975209038513,1.36791350754539));
#10393=CARTESIAN_POINT('Ctrl Pts',(94.2724290749179,1.6813072743529,1.42506906822372));
#10394=CARTESIAN_POINT('Ctrl Pts',(94.2755672257166,1.64397306781175,1.46911624771802));
#10395=CARTESIAN_POINT('Ctrl Pts',(94.2787053765153,1.60495337895619,1.51164034679363));
#10396=CARTESIAN_POINT('Ctrl Pts',(94.281843527314,1.56439099102276,1.55251306828858));
#10397=CARTESIAN_POINT('Ctrl Pts',(94.2858578104481,1.51250409322624,1.60479694088391));
#10398=CARTESIAN_POINT('Ctrl Pts',(94.2898720935823,1.45787927345134,1.6545912562367));
#10399=CARTESIAN_POINT('Ctrl Pts',(94.2938863767164,1.40078855700466,1.70158967397102));
#10400=CARTESIAN_POINT('Ctrl Pts',(94.2978953705898,1.34377306387337,1.74852616610658));
#10401=CARTESIAN_POINT('Ctrl Pts',(94.3019043644632,1.28429848979287,1.79267375274742));
#10402=CARTESIAN_POINT('Ctrl Pts',(94.3059133583366,1.22267430555594,1.83376212812167));
#10403=CARTESIAN_POINT('Ctrl Pts',(94.3099184525911,1.16111006424676,1.87481053611059));
#10404=CARTESIAN_POINT('Ctrl Pts',(94.3139235468457,1.09740076587819,1.91280536170242));
#10405=CARTESIAN_POINT('Ctrl Pts',(94.3179286411002,1.03188823788919,1.94751705114639));
#10406=CARTESIAN_POINT('Ctrl Pts',(94.321931219972,0.966416854769319,1.98220694005903));
#10407=CARTESIAN_POINT('Ctrl Pts',(94.3259337988439,0.899144922756926,2.01361755394063));
#10408=CARTESIAN_POINT('Ctrl Pts',(94.3299363777157,0.830440935359365,2.04156407023622));
#10409=CARTESIAN_POINT('Ctrl Pts',(94.3339394248967,0.76172890946859,2.06951385632575));
#10410=CARTESIAN_POINT('Ctrl Pts',(94.3379424720776,0.691584942794871,2.09399853324094));
#10411=CARTESIAN_POINT('Ctrl Pts',(94.3419455192586,0.620398482558594,2.11488101860105));
#10412=CARTESIAN_POINT('Ctrl Pts',(94.3459485969863,0.549211479107214,2.13576366331282));
#10413=CARTESIAN_POINT('Ctrl Pts',(94.349951674714,0.476982441804223,2.15304393266763));
#10414=CARTESIAN_POINT('Ctrl Pts',(94.3539547524417,0.404114697745888,2.16663502027124));
#10415=CARTESIAN_POINT('Ctrl Pts',(94.3579621228321,0.331168814648818,2.18024068214958));
#10416=CARTESIAN_POINT('Ctrl Pts',(94.3619694932225,0.257583343810738,2.19014918215616));
#10417=CARTESIAN_POINT('Ctrl Pts',(94.3659768636129,0.183769558616102,2.19632528313227));
#10418=CARTESIAN_POINT('Ctrl Pts',(94.3693340446659,0.12193194018719,2.2014993217557));
#10419=CARTESIAN_POINT('Ctrl Pts',(94.3726912257189,0.0599343460611356,
2.20405477785988));
#10420=CARTESIAN_POINT('Ctrl Pts',(94.3760484067719,-0.00198161751640419,
2.20399910916316));
#10421=CARTESIAN_POINT('',(95.1260484068548,0.00109146085463435,2.20399972974436));
#10422=CARTESIAN_POINT('Ctrl Pts',(94.3760484068025,-0.00198161808060188,
2.20399910916266));
#10423=CARTESIAN_POINT('Ctrl Pts',(94.3817549998797,-0.107227419108485,
2.20390448254445));
#10424=CARTESIAN_POINT('Ctrl Pts',(94.3874615929569,-0.212146408604953,
2.19626776901676));
#10425=CARTESIAN_POINT('Ctrl Pts',(94.3931681860342,-0.31586069941933,2.18124918763591));
#10426=CARTESIAN_POINT('Ctrl Pts',(94.3957768718005,-0.363272174278653,
2.17438366227803));
#10427=CARTESIAN_POINT('Ctrl Pts',(94.3983855575668,-0.410432337347612,
2.16597614678547));
#10428=CARTESIAN_POINT('Ctrl Pts',(94.4009942433332,-0.457259089225866,
2.1560450193167));
#10429=CARTESIAN_POINT('Ctrl Pts',(94.4050673082692,-0.530371920063354,
2.14053907851307));
#10430=CARTESIAN_POINT('Ctrl Pts',(94.4091403732052,-0.602836125855812,
2.12128006755923));
#10431=CARTESIAN_POINT('Ctrl Pts',(94.4132134381412,-0.674237480213912,
2.09833739428977));
#10432=CARTESIAN_POINT('Ctrl Pts',(94.4172805189463,-0.745533931983874,
2.07542842830538));
#10433=CARTESIAN_POINT('Ctrl Pts',(94.4213475997513,-0.815770181810802,
2.04884668992764));
#10434=CARTESIAN_POINT('Ctrl Pts',(94.4254146805564,-0.884542825083242,
2.01871245862152));
#10435=CARTESIAN_POINT('Ctrl Pts',(94.4294770029253,-0.953235005180726,
1.98861348400775));
#10436=CARTESIAN_POINT('Ctrl Pts',(94.4335393252941,-1.02046654575262,1.9549704648919));
#10437=CARTESIAN_POINT('Ctrl Pts',(94.437601647663,-1.08585139390071,1.91795274977354));
#10438=CARTESIAN_POINT('Ctrl Pts',(94.4416613918023,-1.15119474432084,1.88095852864676));
#10439=CARTESIAN_POINT('Ctrl Pts',(94.4457211359416,-1.2146933136601,1.84059409635276));
#10440=CARTESIAN_POINT('Ctrl Pts',(94.4497808800809,-1.2759843737873,1.79707536788267));
#10441=CARTESIAN_POINT('Ctrl Pts',(94.453839359536,-1.33725634063282,1.75357019628922));
#10442=CARTESIAN_POINT('Ctrl Pts',(94.457897838991,-1.39632177457106,1.70691295571196));
#10443=CARTESIAN_POINT('Ctrl Pts',(94.4619563184461,-1.45284710892216,1.65736274789091));
#10444=CARTESIAN_POINT('Ctrl Pts',(94.4660148450784,-1.50937310034565,1.60781196407905));
#10445=CARTESIAN_POINT('Ctrl Pts',(94.4700733717108,-1.5633585756961,1.55536846233581));
#10446=CARTESIAN_POINT('Ctrl Pts',(94.4741318983432,-1.61450446676175,1.50033040587943));
#10447=CARTESIAN_POINT('Ctrl Pts',(94.4781945753283,-1.66570266091831,1.44523606610469));
#10448=CARTESIAN_POINT('Ctrl Pts',(94.4822572523134,-1.71405514626068,1.38754222374569));
#10449=CARTESIAN_POINT('Ctrl Pts',(94.4863199292985,-1.7593015726799,1.32758200363143));
#10450=CARTESIAN_POINT('Ctrl Pts',(94.4903847282755,-1.80457163192863,1.26759046547126));
#10451=CARTESIAN_POINT('Ctrl Pts',(94.4944495272525,-1.84673213356332,1.20533058792501));
#10452=CARTESIAN_POINT('Ctrl Pts',(94.4985143262296,-1.88556623555352,1.14116430514652));
#10453=CARTESIAN_POINT('Ctrl Pts',(94.5025863864716,-1.92446970990525,1.07688339717164));
#10454=CARTESIAN_POINT('Ctrl Pts',(94.5066584467136,-1.96003468920312,1.01068970284516));
#10455=CARTESIAN_POINT('Ctrl Pts',(94.5107305069556,-1.9920906561783,0.942969149849091));
#10456=CARTESIAN_POINT('Ctrl Pts',(94.5138686577544,-2.01679472546827,0.890780013428237));
#10457=CARTESIAN_POINT('Ctrl Pts',(94.5170068085533,-2.03941571223733,0.837684570322939));
#10458=CARTESIAN_POINT('Ctrl Pts',(94.5201449593522,-2.05989571383001,0.78386583555145));
#10459=CARTESIAN_POINT('Ctrl Pts',(94.5242180242882,-2.08647709303151,0.714013487609342));
#10460=CARTESIAN_POINT('Ctrl Pts',(94.5282910892241,-2.1095526001422,0.642672814808761));
#10461=CARTESIAN_POINT('Ctrl Pts',(94.5323641541601,-2.1289561356839,0.570229578620661));
#10462=CARTESIAN_POINT('Ctrl Pts',(94.5364312349652,-2.14833116362775,0.497892775749264));
#10463=CARTESIAN_POINT('Ctrl Pts',(94.5404983157703,-2.164044808468,0.424457082991674));
#10464=CARTESIAN_POINT('Ctrl Pts',(94.5445653965753,-2.17597959149856,0.350326729470851));
#10465=CARTESIAN_POINT('Ctrl Pts',(94.5486277189442,-2.18790041097486,0.276283107582392));
#10466=CARTESIAN_POINT('Ctrl Pts',(94.5526900413131,-2.19605107709203,0.201546908690907));
#10467=CARTESIAN_POINT('Ctrl Pts',(94.556752363682,-2.20036475489787,0.126534364515138));
#10468=CARTESIAN_POINT('Ctrl Pts',(94.5608121078213,-2.20467569494667,0.0515694284663048));
#10469=CARTESIAN_POINT('Ctrl Pts',(94.5648718519606,-2.20515445176705,-0.0236710293636508));
#10470=CARTESIAN_POINT('Ctrl Pts',(94.5689315960999,-2.20178596711089,-0.0987651509065199));
#10471=CARTESIAN_POINT('Ctrl Pts',(94.572990075555,-2.19841853179905,-0.173835879262582));
#10472=CARTESIAN_POINT('Ctrl Pts',(94.57704855501,-2.19120625593485,-0.248759885171571));
#10473=CARTESIAN_POINT('Ctrl Pts',(94.5811070344651,-2.18018617975546,-0.323116421129124));
#10474=CARTESIAN_POINT('Ctrl Pts',(94.5851655610975,-2.16916597547443,-0.397473821435904));
#10475=CARTESIAN_POINT('Ctrl Pts',(94.5892240877299,-2.15433795476321,-0.47126326665469));
#10476=CARTESIAN_POINT('Ctrl Pts',(94.5932826143623,-2.13579068078345,-0.544071840732983));
#10477=CARTESIAN_POINT('Ctrl Pts',(94.5973452913474,-2.11722443988891,-0.616954870713584));
#10478=CARTESIAN_POINT('Ctrl Pts',(94.6014079683325,-2.09493146867303,-0.688854562780362));
#10479=CARTESIAN_POINT('Ctrl Pts',(94.6054706453176,-2.06905069359172,-0.759371600303586));
#10480=CARTESIAN_POINT('Ctrl Pts',(94.6095354442947,-2.04315640062639,-0.829925469843297));
#10481=CARTESIAN_POINT('Ctrl Pts',(94.6136002432717,-2.01367075939374,-0.899094807061877));
#10482=CARTESIAN_POINT('Ctrl Pts',(94.6176650422488,-1.98078048399045,-0.966501254133985));
#10483=CARTESIAN_POINT('Ctrl Pts',(94.6217371024908,-1.947831454143,-1.03402811455874));
#10484=CARTESIAN_POINT('Ctrl Pts',(94.6258091627328,-1.91146587328994,-1.09978537613696));
#10485=CARTESIAN_POINT('Ctrl Pts',(94.6298812229749,-1.87191572165627,-1.16342061655108));
#10486=CARTESIAN_POINT('Ctrl Pts',(94.6330193737737,-1.84143622661748,-1.21246138919992));
#10487=CARTESIAN_POINT('Ctrl Pts',(94.6361575245726,-1.80906632918666,-1.26024239862049));
#10488=CARTESIAN_POINT('Ctrl Pts',(94.6392956753715,-1.77492847957935,-1.30661581667226));
#10489=CARTESIAN_POINT('Ctrl Pts',(94.6433687403075,-1.7306203225984,-1.36680474803195));
#10490=CARTESIAN_POINT('Ctrl Pts',(94.6474418052434,-1.68316168372401,-1.42485341916433));
#10491=CARTESIAN_POINT('Ctrl Pts',(94.6515148701794,-1.6327867971314,-1.48041321093585));
#10492=CARTESIAN_POINT('Ctrl Pts',(94.6555819509845,-1.58248592112336,-1.53589137448057));
#10493=CARTESIAN_POINT('Ctrl Pts',(94.6596490317896,-1.5292776220016,-1.58888756782984));
#10494=CARTESIAN_POINT('Ctrl Pts',(94.6637161125946,-1.47343799962834,-1.63908403117449));
#10495=CARTESIAN_POINT('Ctrl Pts',(94.6677784349635,-1.41766370894944,-1.68922176525376));
#10496=CARTESIAN_POINT('Ctrl Pts',(94.6718407573323,-1.35926456482471,-1.73656595970663));
#10497=CARTESIAN_POINT('Ctrl Pts',(94.6759030797012,-1.2985541950541,-1.78083491725298));
#10498=CARTESIAN_POINT('Ctrl Pts',(94.6799628238405,-1.2378823562655,-1.82507577866988));
#10499=CARTESIAN_POINT('Ctrl Pts',(94.6840225679798,-1.17490258747322,-1.86624499563372));
#10500=CARTESIAN_POINT('Ctrl Pts',(94.6880823121191,-1.10996129907252,-1.90410134041265));
#10501=CARTESIAN_POINT('Ctrl Pts',(94.6921407915742,-1.04504024106613,-1.94194589225059));
#10502=CARTESIAN_POINT('Ctrl Pts',(94.6961992710292,-0.978159288886569,
-1.97647938063708));
#10503=CARTESIAN_POINT('Ctrl Pts',(94.7002577504843,-0.909692147535444,
-2.00750496804176));
#10504=CARTESIAN_POINT('Ctrl Pts',(94.7043162771167,-0.841224210295729,
-2.0385309160999));
#10505=CARTESIAN_POINT('Ctrl Pts',(94.708374803749,-0.771170482907496,-2.06604868677474));
#10506=CARTESIAN_POINT('Ctrl Pts',(94.7124333303814,-0.699926004260587,
-2.08990899049691));
#10507=CARTESIAN_POINT('Ctrl Pts',(94.7164960073665,-0.628608669195191,
-2.1137936943734));
#10508=CARTESIAN_POINT('Ctrl Pts',(94.7205586843516,-0.556098604959127,
-2.13401331032924));
#10509=CARTESIAN_POINT('Ctrl Pts',(94.7246213613367,-0.482806708072885,
-2.15046824729867));
#10510=CARTESIAN_POINT('Ctrl Pts',(94.7286861603137,-0.409476529823017,
-2.16693177890752));
#10511=CARTESIAN_POINT('Ctrl Pts',(94.7327509592908,-0.335364176754445,
-2.17962663506225));
#10512=CARTESIAN_POINT('Ctrl Pts',(94.7368157582678,-0.260888821958733,
-2.18850474584292));
#10513=CARTESIAN_POINT('Ctrl Pts',(94.7408878185098,-0.186280426073485,
-2.19739871627991));
#10514=CARTESIAN_POINT('Ctrl Pts',(94.7449598787518,-0.11130821029882,-2.20246229040065));
#10515=CARTESIAN_POINT('Ctrl Pts',(94.7490319389938,-0.0363940751997966,
-2.20369949659439));
#10516=CARTESIAN_POINT('Ctrl Pts',(94.7521700897927,0.0213388263136973,
-2.20465295488688));
#10517=CARTESIAN_POINT('Ctrl Pts',(94.7553082405916,0.0790371629527067,
-2.20333497533854));
#10518=CARTESIAN_POINT('Ctrl Pts',(94.7584463913905,0.136510339980724,-2.19976838032515));
#10519=CARTESIAN_POINT('Ctrl Pts',(94.7625194563265,0.211105857250251,-2.19513922958611));
#10520=CARTESIAN_POINT('Ctrl Pts',(94.7665925212625,0.28560949395828,-2.18670248013346));
#10521=CARTESIAN_POINT('Ctrl Pts',(94.7706655861985,0.359601324857395,-2.17446611543174));
#10522=CARTESIAN_POINT('Ctrl Pts',(94.7747326670035,0.43348444725053,-2.16224772834876));
#10523=CARTESIAN_POINT('Ctrl Pts',(94.7787997478086,0.506856789596386,-2.14624088657335));
#10524=CARTESIAN_POINT('Ctrl Pts',(94.7828668286137,0.579301680042337,-2.12650548165297));
#10525=CARTESIAN_POINT('Ctrl Pts',(94.7869291509825,0.651661810827729,-2.10679316692173));
#10526=CARTESIAN_POINT('Ctrl Pts',(94.7909914733514,0.723096187216718,-2.0833610809537));
#10527=CARTESIAN_POINT('Ctrl Pts',(94.7950537957203,0.79319811429643,-2.05632019672924));
#10528=CARTESIAN_POINT('Ctrl Pts',(94.7991135398596,0.863255549865023,-2.02929647451232));
#10529=CARTESIAN_POINT('Ctrl Pts',(94.8031732839989,0.931981769914055,-1.99866867047218));
#10530=CARTESIAN_POINT('Ctrl Pts',(94.8072330281382,0.998986331668492,-1.9645972384027));
#10531=CARTESIAN_POINT('Ctrl Pts',(94.8112915075933,1.06597002028138,-1.93053642020497));
#10532=CARTESIAN_POINT('Ctrl Pts',(94.8153499870483,1.13123269013548,-1.89303432015572));
#10533=CARTESIAN_POINT('Ctrl Pts',(94.8194084665034,1.19440641938499,-1.85229838452986));
#10534=CARTESIAN_POINT('Ctrl Pts',(94.8234669931358,1.25758088299038,-1.81156197537371));
#10535=CARTESIAN_POINT('Ctrl Pts',(94.8275255197682,1.31866595747844,-1.76759191625749));
#10536=CARTESIAN_POINT('Ctrl Pts',(94.8315840464006,1.37732212565063,-1.72063934692696));
#10537=CARTESIAN_POINT('Ctrl Pts',(94.8356467233857,1.43603827711441,-1.6736387627031));
#10538=CARTESIAN_POINT('Ctrl Pts',(94.8397094003708,1.49232018855618,-1.62364987664444));
#10539=CARTESIAN_POINT('Ctrl Pts',(94.8437720773559,1.54586152209201,-1.57096408441294));
#10540=CARTESIAN_POINT('Ctrl Pts',(94.8478368763329,1.59943082100116,-1.51825077366908));
#10541=CARTESIAN_POINT('Ctrl Pts',(94.85190167531,1.65025636839036,-1.46283810379346));
#10542=CARTESIAN_POINT('Ctrl Pts',(94.855966474287,1.69807064518424,-1.40505234207256));
#10543=CARTESIAN_POINT('Ctrl Pts',(94.8600385345291,1.74597033632085,-1.34716335317376));
#10544=CARTESIAN_POINT('Ctrl Pts',(94.8641105947711,1.79084772662142,-1.28689318840831));
#10545=CARTESIAN_POINT('Ctrl Pts',(94.8681826550131,1.83247760753661,-1.22459863542178));
#10546=CARTESIAN_POINT('Ctrl Pts',(94.871320805812,1.8645598549217,-1.17659106932453));
#10547=CARTESIAN_POINT('Ctrl Pts',(94.8744589566109,1.8947142439976,-1.12738184315265));
#10548=CARTESIAN_POINT('Ctrl Pts',(94.8775971074097,1.92285668869812,-1.0771435163101));
#10549=CARTESIAN_POINT('Ctrl Pts',(94.8816701723457,1.95938329690438,-1.01193824715018));
#10550=CARTESIAN_POINT('Ctrl Pts',(94.8857432372817,1.99265985766841,-0.944747167922621));
#10551=CARTESIAN_POINT('Ctrl Pts',(94.8898163022177,2.02246555692644,-0.875927548970939));
#10552=CARTESIAN_POINT('Ctrl Pts',(94.8938833830228,2.05222746576875,-0.807209039531793));
#10553=CARTESIAN_POINT('Ctrl Pts',(94.8979504638278,2.07852844926698,-0.736867175240501));
#10554=CARTESIAN_POINT('Ctrl Pts',(94.9020175446329,2.10119308455649,-0.665284616846028));
#10555=CARTESIAN_POINT('Ctrl Pts',(94.9060798670018,2.12383120249215,-0.59378580919392));
#10556=CARTESIAN_POINT('Ctrl Pts',(94.9101421893706,2.14284128150927,-0.52104964433311));
#10557=CARTESIAN_POINT('Ctrl Pts',(94.9142045117395,2.15809623810248,-0.447478074421437));
#10558=CARTESIAN_POINT('Ctrl Pts',(94.9182642558788,2.17334151284958,-0.373953198095192));
#10559=CARTESIAN_POINT('Ctrl Pts',(94.9223240000181,2.18483629780017,-0.29959443518531));
#10560=CARTESIAN_POINT('Ctrl Pts',(94.9263837441574,2.19250390352807,-0.224816887742446));
#10561=CARTESIAN_POINT('Ctrl Pts',(94.9304422236125,2.2001691206571,-0.150062634867785));
#10562=CARTESIAN_POINT('Ctrl Pts',(94.9345007030675,2.20400947702594,-0.0748903311412995));
#10563=CARTESIAN_POINT('Ctrl Pts',(94.9385591825226,2.20399998241828,0.000278388606040127));
#10564=CARTESIAN_POINT('Ctrl Pts',(94.942617709155,2.20399048770026,0.0754479821437415));
#10565=CARTESIAN_POINT('Ctrl Pts',(94.9466762357873,2.20013105500196,0.150613514159087));
#10566=CARTESIAN_POINT('Ctrl Pts',(94.9507347624197,2.1924488084373,0.225353549743164));
#10567=CARTESIAN_POINT('Ctrl Pts',(94.9547974394048,2.18475870581164,0.30017001639128));
#10568=CARTESIAN_POINT('Ctrl Pts',(94.9588601163899,2.17323803158467,0.374559641677874));
#10569=CARTESIAN_POINT('Ctrl Pts',(94.962922793375,2.15796572196852,0.448107066234035));
#10570=CARTESIAN_POINT('Ctrl Pts',(94.9669875923521,2.14268543541547,0.521692905619417));
#10571=CARTESIAN_POINT('Ctrl Pts',(94.9710523913291,2.12364973224626,0.594435205933648));
#10572=CARTESIAN_POINT('Ctrl Pts',(94.9751171903062,2.10098789089885,0.665932340629578));
#10573=CARTESIAN_POINT('Ctrl Pts',(94.9791892505482,2.07828556695056,0.737557196190026));
#10574=CARTESIAN_POINT('Ctrl Pts',(94.9832613107902,2.05194433384007,0.807931995367446));
#10575=CARTESIAN_POINT('Ctrl Pts',(94.9873333710322,2.022142046902,0.876674136809688));
#10576=CARTESIAN_POINT('Ctrl Pts',(94.9904715218311,1.99917478585852,0.929650564775497));
#10577=CARTESIAN_POINT('Ctrl Pts',(94.9936096726299,1.97415298327347,0.981657723094009));
#10578=CARTESIAN_POINT('Ctrl Pts',(94.9967478234288,1.9471761147697,1.0325314416861));
#10579=CARTESIAN_POINT('Ctrl Pts',(95.0008208883648,1.91216232982829,1.09856139774659));
#10580=CARTESIAN_POINT('Ctrl Pts',(95.0048939533008,1.87371854060252,1.16293566041432));
#10581=CARTESIAN_POINT('Ctrl Pts',(95.0089670182368,1.83202538915432,1.22527506034113));
#10582=CARTESIAN_POINT('Ctrl Pts',(95.0130340990418,1.79039349311968,1.28752287146761));
#10583=CARTESIAN_POINT('Ctrl Pts',(95.0171011798469,1.74552197633398,1.34774136186964));
#10584=CARTESIAN_POINT('Ctrl Pts',(95.0211682606519,1.6976374152314,1.40557575619618));
#10585=CARTESIAN_POINT('Ctrl Pts',(95.0252305830208,1.64980887849607,1.46334248496888));
#10586=CARTESIAN_POINT('Ctrl Pts',(95.0292929053897,1.59897460422833,1.51873029357842));
#10587=CARTESIAN_POINT('Ctrl Pts',(95.0333552277586,1.54540357443698,1.57141458314393));
#10588=CARTESIAN_POINT('Ctrl Pts',(95.0374149718979,1.4918665445108,1.62406543563069));
#10589=CARTESIAN_POINT('Ctrl Pts',(95.0414747160372,1.43559654537654,1.67401584003322));
#10590=CARTESIAN_POINT('Ctrl Pts',(95.0455344601765,1.37690091599836,1.72097642852041));
#10591=CARTESIAN_POINT('Ctrl Pts',(95.0495929396315,1.3182235713779,1.76792238792889));
#10592=CARTESIAN_POINT('Ctrl Pts',(95.0536514190866,1.25712246935887,1.81188008255283));
#10593=CARTESIAN_POINT('Ctrl Pts',(95.0577098985416,1.19393845136267,1.85260005785321));
#10594=CARTESIAN_POINT('Ctrl Pts',(95.061768425174,1.13075369889094,1.89332050649837));
#10595=CARTESIAN_POINT('Ctrl Pts',(95.0658269518064,1.06548638467391,1.93080290395108));
#10596=CARTESIAN_POINT('Ctrl Pts',(95.0698854784388,0.9985054187136,1.9648417057869));
#10597=CARTESIAN_POINT('Ctrl Pts',(95.0739481554239,0.931455956311528,1.99891531656843));
#10598=CARTESIAN_POINT('Ctrl Pts',(95.078010832409,0.862689769272217,2.02953808269096));
#10599=CARTESIAN_POINT('Ctrl Pts',(95.0820735093941,0.792598733999952,2.05655129935085));
#10600=CARTESIAN_POINT('Ctrl Pts',(95.0861383083712,0.722471089217977,2.08357862538455));
#10601=CARTESIAN_POINT('Ctrl Pts',(95.0902031073482,0.651017672324267,2.10699249871576));
#10602=CARTESIAN_POINT('Ctrl Pts',(95.0942679063253,0.57864609381734,2.12668396761483));
#10603=CARTESIAN_POINT('Ctrl Pts',(95.0983399665673,0.506145232359268,2.14641061290861));
#10604=CARTESIAN_POINT('Ctrl Pts',(95.1024120268093,0.432723400366107,2.16240146991543));
#10605=CARTESIAN_POINT('Ctrl Pts',(95.1064840870513,0.358798537729981,2.17459872374717));
#10606=CARTESIAN_POINT('Ctrl Pts',(95.1096222378502,0.301828023309634,2.18399859005102));
#10607=CARTESIAN_POINT('Ctrl Pts',(95.1127603886491,0.244558981630548,2.19114645589506));
#10608=CARTESIAN_POINT('Ctrl Pts',(95.1158985394479,0.187183294628014,2.19603697924516));
#10609=CARTESIAN_POINT('Ctrl Pts',(95.1192818285661,0.12532567530837,2.20130952842877));
#10610=CARTESIAN_POINT('Ctrl Pts',(95.1226651176843,0.0632421790914876,
2.2039689515483));
#10611=CARTESIAN_POINT('Ctrl Pts',(95.1260484068025,0.00109146181604489,
2.20399972974388));
#10612=CARTESIAN_POINT('',(95.8760484067755,0.00133902696002769,2.20399959324107));
#10613=CARTESIAN_POINT('Ctrl Pts',(95.1260484068548,0.00109146085464169,
2.20399972974436));
#10614=CARTESIAN_POINT('Ctrl Pts',(95.1300735385946,-0.072849847740999,
2.20403634682865));
#10615=CARTESIAN_POINT('Ctrl Pts',(95.1340986703343,-0.146942092471922,
2.20034777635078));
#10616=CARTESIAN_POINT('Ctrl Pts',(95.138123802074,-0.220773424115571,2.19291474873153));
#10617=CARTESIAN_POINT('Ctrl Pts',(95.1421623626321,-0.294851075035982,
2.18545692272457));
#10618=CARTESIAN_POINT('Ctrl Pts',(95.1462009231901,-0.368665574139318,
2.17422954668617));
#10619=CARTESIAN_POINT('Ctrl Pts',(95.1502394837482,-0.441799140599636,
2.15926596772269));
#10620=CARTESIAN_POINT('Ctrl Pts',(95.1542550801847,-0.514516853915588,
2.14438747487855));
#10621=CARTESIAN_POINT('Ctrl Pts',(95.1582706766213,-0.586560870724673,
2.12581523600944));
#10622=CARTESIAN_POINT('Ctrl Pts',(95.1622862730578,-0.657526071900074,
2.10363387136917));
#10623=CARTESIAN_POINT('Ctrl Pts',(95.1662998439655,-0.728455477133412,
2.08146369535136));
#10624=CARTESIAN_POINT('Ctrl Pts',(95.1703134148733,-0.798306679744222,
2.0556881501414));
#10625=CARTESIAN_POINT('Ctrl Pts',(95.1743269857811,-0.866687961998495,
2.02644219669027));
#10626=CARTESIAN_POINT('Ctrl Pts',(95.178339900323,-0.935058061409059,1.9972010260235));
#10627=CARTESIAN_POINT('Ctrl Pts',(95.1823528148649,-1.00195826810386,1.96449076691085));
#10628=CARTESIAN_POINT('Ctrl Pts',(95.1863657294069,-1.06701681521606,1.92849452061606));
#10629=CARTESIAN_POINT('Ctrl Pts',(95.1904226899119,-1.1327894483958,1.89210317761064));
#10630=CARTESIAN_POINT('Ctrl Pts',(95.1944796504169,-1.19667928584886,1.85235349304124));
#10631=CARTESIAN_POINT('Ctrl Pts',(95.1985366109219,-1.25832955190855,1.8094813452461));
#10632=CARTESIAN_POINT('Ctrl Pts',(95.202554691631,-1.31938899393611,1.76702006178043));
#10633=CARTESIAN_POINT('Ctrl Pts',(95.2065727723401,-1.37825125334203,1.72149626042148));
#10634=CARTESIAN_POINT('Ctrl Pts',(95.2105908530492,-1.43460238853593,1.6731802015345));
#10635=CARTESIAN_POINT('Ctrl Pts',(95.2146672534522,-1.49177142192389,1.62416286809161));
#10636=CARTESIAN_POINT('Ctrl Pts',(95.2187436538552,-1.54635547126111,1.57227192882445));
#10637=CARTESIAN_POINT('Ctrl Pts',(95.2228200542582,-1.59806652092165,1.51782719527269));
#10638=CARTESIAN_POINT('Ctrl Pts',(95.2268964546612,-1.6497775705822,1.46338246172093));
#10639=CARTESIAN_POINT('Ctrl Pts',(95.2309728550642,-1.698615337954,1.40638437361926));
#10640=CARTESIAN_POINT('Ctrl Pts',(95.2350492554671,-1.74433661151164,1.34718439188557));
#10641=CARTESIAN_POINT('Ctrl Pts',(95.2391223204031,-1.79002047417145,1.28803284984519));
#10642=CARTESIAN_POINT('Ctrl Pts',(95.2431953853391,-1.83278022606828,1.22644085164921));
#10643=CARTESIAN_POINT('Ctrl Pts',(95.2472684502751,-1.87234510209011,1.16272946925723));
#10644=CARTESIAN_POINT('Ctrl Pts',(95.2513355310802,-1.91185184955223,1.09911169137681));
#10645=CARTESIAN_POINT('Ctrl Pts',(95.2554026118852,-1.94817279064879,1.03338111369175));
#10646=CARTESIAN_POINT('Ctrl Pts',(95.2594696926903,-1.981078342687,0.965890573583024));
#10647=CARTESIAN_POINT('Ctrl Pts',(95.2635320150592,-2.0139453956205,0.89847899660389));
#10648=CARTESIAN_POINT('Ctrl Pts',(95.2675943374281,-2.04340479037228,0.829311975244283));
#10649=CARTESIAN_POINT('Ctrl Pts',(95.2716566597969,-2.0692719364077,0.758768510940943));
#10650=CARTESIAN_POINT('Ctrl Pts',(95.2757164039363,-2.09512266537068,0.688269818378645));
#10651=CARTESIAN_POINT('Ctrl Pts',(95.2797761480756,-2.11738550585129,0.616396863546591));
#10652=CARTESIAN_POINT('Ctrl Pts',(95.2838358922149,-2.1359237916369,0.543549037640074));
#10653=CARTESIAN_POINT('Ctrl Pts',(95.2878943716699,-2.15445630240879,0.470723905158345));
#10654=CARTESIAN_POINT('Ctrl Pts',(95.291952851125,-2.16926644447123,0.39692496697706));
#10655=CARTESIAN_POINT('Ctrl Pts',(95.29601133058,-2.18026773625882,0.322565649486823));
#10656=CARTESIAN_POINT('Ctrl Pts',(95.3000698572124,-2.19126915592969,0.248205467614994));
#10657=CARTESIAN_POINT('Ctrl Pts',(95.3041283838449,-2.19846156931004,0.173285366082212));
#10658=CARTESIAN_POINT('Ctrl Pts',(95.3081869104772,-2.20181007632792,0.0982262071996763));
#10659=CARTESIAN_POINT('Ctrl Pts',(95.3122495874623,-2.20516200761437,0.0230902909095669));
#10660=CARTESIAN_POINT('Ctrl Pts',(95.3163122644474,-2.20466216147588,-0.0521844886567871));
#10661=CARTESIAN_POINT('Ctrl Pts',(95.3203749414325,-2.20032778102013,-0.127175689780132));
#10662=CARTESIAN_POINT('Ctrl Pts',(95.3244397404096,-2.19599113665797,-0.202206059837059));
#10663=CARTESIAN_POINT('Ctrl Pts',(95.3285045393866,-2.18781602149744,-0.276952081418629));
#10664=CARTESIAN_POINT('Ctrl Pts',(95.3325693383637,-2.17587148944344,-0.350997523391801));
#10665=CARTESIAN_POINT('Ctrl Pts',(95.3366413986057,-2.16390561994752,-0.42517523846793));
#10666=CARTESIAN_POINT('Ctrl Pts',(95.3407134588477,-2.14815698392865,-0.49864940661286));
#10667=CARTESIAN_POINT('Ctrl Pts',(95.3447855190897,-2.12874547502596,-0.571015501152542));
#10668=CARTESIAN_POINT('Ctrl Pts',(95.3479236698886,-2.11378591191795,-0.626784744212076));
#10669=CARTESIAN_POINT('Ctrl Pts',(95.3510618206874,-2.09665198995791,-0.68189612088876));
#10670=CARTESIAN_POINT('Ctrl Pts',(95.3541999714863,-2.07741806422642,-0.736172660743221));
#10671=CARTESIAN_POINT('Ctrl Pts',(95.3582730364223,-2.05245399031801,-0.806619202511925));
#10672=CARTESIAN_POINT('Ctrl Pts',(95.3623461013583,-2.02385438390514,-0.875930335362855));
#10673=CARTESIAN_POINT('Ctrl Pts',(95.3664191662942,-1.99174239801431,-0.943704519408594));
#10674=CARTESIAN_POINT('Ctrl Pts',(95.3704862470993,-1.95967759092642,-1.01137912989062));
#10675=CARTESIAN_POINT('Ctrl Pts',(95.3745533279044,-1.92411085254978,-1.0775208468792));
#10676=CARTESIAN_POINT('Ctrl Pts',(95.3786204087094,-1.88521434804376,-1.14174553291439));
#10677=CARTESIAN_POINT('Ctrl Pts',(95.3826827310783,-1.8463633519856,-1.20589507683043));
#10678=CARTESIAN_POINT('Ctrl Pts',(95.3867450534472,-1.80419057593485,-1.26813163958155));
#10679=CARTESIAN_POINT('Ctrl Pts',(95.390807375816,-1.75891455346316,-1.32809472313367));
#10680=CARTESIAN_POINT('Ctrl Pts',(95.3948671199553,-1.71366726627367,-1.38801974998305));
#10681=CARTESIAN_POINT('Ctrl Pts',(95.3989268640946,-1.66532092797137,-1.44567378085091));
#10682=CARTESIAN_POINT('Ctrl Pts',(95.4029866082339,-1.61413717598334,-1.50072555022847));
#10683=CARTESIAN_POINT('Ctrl Pts',(95.407045087689,-1.56296936866645,-1.55576016997701));
#10684=CARTESIAN_POINT('Ctrl Pts',(95.411103567144,-1.50896622751712,-1.60819378830145));
#10685=CARTESIAN_POINT('Ctrl Pts',(95.4151620465991,-1.45242837753489,-1.65772971504144));
#10686=CARTESIAN_POINT('Ctrl Pts',(95.4192205732315,-1.39588987033482,-1.70726621760621));
#10687=CARTESIAN_POINT('Ctrl Pts',(95.4232790998638,-1.33681695610085,-1.75390464840955));
#10688=CARTESIAN_POINT('Ctrl Pts',(95.4273376264962,-1.27554445759278,-1.79738764230322));
#10689=CARTESIAN_POINT('Ctrl Pts',(95.4314003034813,-1.21420930026703,-1.84091510301403));
#10690=CARTESIAN_POINT('Ctrl Pts',(95.4354629804664,-1.15067045708161,-1.88128040607972));
#10691=CARTESIAN_POINT('Ctrl Pts',(95.4395256574515,-1.08529233052476,-1.91826915663682));
#10692=CARTESIAN_POINT('Ctrl Pts',(95.4435904564286,-1.01988005607513,-1.95527722692599));
#10693=CARTESIAN_POINT('Ctrl Pts',(95.4476552554056,-0.952627012595539,
-1.98890501889766));
#10694=CARTESIAN_POINT('Ctrl Pts',(95.4517200543827,-0.883920454766032,
-2.0189850493865));
#10695=CARTESIAN_POINT('Ctrl Pts',(95.4557921146247,-0.815091161095456,
-2.04911881416153));
#10696=CARTESIAN_POINT('Ctrl Pts',(95.4598641748667,-0.744803613989299,
-2.07569198941107));
#10697=CARTESIAN_POINT('Ctrl Pts',(95.4639362351087,-0.673462776609276,
-2.0985861641881));
#10698=CARTESIAN_POINT('Ctrl Pts',(95.4670743859076,-0.618483652404165,
-2.11622965878202));
#10699=CARTESIAN_POINT('Ctrl Pts',(95.4702125367064,-0.562879348821488,
-2.13168917184189));
#10700=CARTESIAN_POINT('Ctrl Pts',(95.4733506875053,-0.506838895599709,
-2.14493131216533));
#10701=CARTESIAN_POINT('Ctrl Pts',(95.4774237524413,-0.434102937500836,
-2.16211853511467));
#10702=CARTESIAN_POINT('Ctrl Pts',(95.4814968173773,-0.360351477878771,
-2.17563492618856));
#10703=CARTESIAN_POINT('Ctrl Pts',(95.4855698823133,-0.285988735521359,
-2.18536643223851));
#10704=CARTESIAN_POINT('Ctrl Pts',(95.4896369631183,-0.2117352466116,-2.19508364079818));
#10705=CARTESIAN_POINT('Ctrl Pts',(95.4937040439234,-0.136872727543854,
-2.20102694322759));
#10706=CARTESIAN_POINT('Ctrl Pts',(95.4977711247285,-0.0618173262461914,
-2.20313290978456));
#10707=CARTESIAN_POINT('Ctrl Pts',(95.5018334470973,0.0131502611242621,
-2.20523641238569));
#10708=CARTESIAN_POINT('Ctrl Pts',(95.5058957694662,0.0883098074955325,
-2.20351148567463));
#10709=CARTESIAN_POINT('Ctrl Pts',(95.5099580918351,0.163239910382419,-2.19794648061738));
#10710=CARTESIAN_POINT('Ctrl Pts',(95.5140178359744,0.238122457465352,-2.19238500749562));
#10711=CARTESIAN_POINT('Ctrl Pts',(95.5180775801137,0.31277537508975,-2.18298832761805));
#10712=CARTESIAN_POINT('Ctrl Pts',(95.522137324253,0.386778475984921,-2.16979685927388));
#10713=CARTESIAN_POINT('Ctrl Pts',(95.5261958037081,0.460758523566107,-2.1566095003124));
#10714=CARTESIAN_POINT('Ctrl Pts',(95.5302542831632,0.534088686589196,-2.13962978371868));
#10715=CARTESIAN_POINT('Ctrl Pts',(95.5343127626182,0.606356713896499,-2.11894963024434));
#10716=CARTESIAN_POINT('Ctrl Pts',(95.5383712892506,0.678625581275309,-2.0982692363759));
#10717=CARTESIAN_POINT('Ctrl Pts',(95.542429815883,0.749831829880887,-2.07388845329947));
#10718=CARTESIAN_POINT('Ctrl Pts',(95.5464883425154,0.819577731951936,-2.04594925188493));
#10719=CARTESIAN_POINT('Ctrl Pts',(95.5505510195005,0.8893949579589,-2.01798147913141));
#10720=CARTESIAN_POINT('Ctrl Pts',(95.5546136964856,0.957748411015381,-1.98644819924844));
#10721=CARTESIAN_POINT('Ctrl Pts',(95.5586763734707,1.02426045273147,-1.9515395268788));
#10722=CARTESIAN_POINT('Ctrl Pts',(95.5627411724478,1.09080723459977,-1.91661262123049));
#10723=CARTESIAN_POINT('Ctrl Pts',(95.5668059714248,1.15551027856716,-1.87830705568835));
#10724=CARTESIAN_POINT('Ctrl Pts',(95.5708707704018,1.21801899346771,-1.8368575697511));
#10725=CARTESIAN_POINT('Ctrl Pts',(95.5749428306438,1.28063937252291,-1.79533403938956));
#10726=CARTESIAN_POINT('Ctrl Pts',(95.5790148908859,1.34105720834959,-1.75065565496199));
#10727=CARTESIAN_POINT('Ctrl Pts',(95.5830869511279,1.39895355987823,-1.70309862817866));
#10728=CARTESIAN_POINT('Ctrl Pts',(95.5862251019268,1.44357163304115,-1.66644860025108));
#10729=CARTESIAN_POINT('Ctrl Pts',(95.5893632527256,1.48669281739357,-1.62808978664815));
#10730=CARTESIAN_POINT('Ctrl Pts',(95.5925014035245,1.52818662763047,-1.58816297373141));
#10731=CARTESIAN_POINT('Ctrl Pts',(95.5965744684605,1.58204222424386,-1.53634121240784));
#10732=CARTESIAN_POINT('Ctrl Pts',(95.6006475333965,1.63336272749686,-1.48167699586817));
#10733=CARTESIAN_POINT('Ctrl Pts',(95.6047205983325,1.68183326234142,-1.42444827132543));
#10734=CARTESIAN_POINT('Ctrl Pts',(95.6087876791376,1.73023258446756,-1.36730362699884));
#10735=CARTESIAN_POINT('Ctrl Pts',(95.6128547599426,1.77578994538915,-1.30760231653738));
#10736=CARTESIAN_POINT('Ctrl Pts',(95.6169218407477,1.81822655528487,-1.24565974232811));
#10737=CARTESIAN_POINT('Ctrl Pts',(95.6209841631166,1.86061351485146,-1.18378964019433));
#10738=CARTESIAN_POINT('Ctrl Pts',(95.6250464854854,1.89988670908004,-1.11968387603866));
#10739=CARTESIAN_POINT('Ctrl Pts',(95.6291088078543,1.93580802250771,-1.05369032452367));
#10740=CARTESIAN_POINT('Ctrl Pts',(95.6331685519936,1.97170653779581,-0.987738657061754));
#10741=CARTESIAN_POINT('Ctrl Pts',(95.6372282961329,2.00425716606191,-0.919901998078399));
#10742=CARTESIAN_POINT('Ctrl Pts',(95.6412880402722,2.03326621255493,-0.850555412000014));
#10743=CARTESIAN_POINT('Ctrl Pts',(95.6453465197272,2.06226622220153,-0.781230428646454));
#10744=CARTESIAN_POINT('Ctrl Pts',(95.6494049991823,2.08772665642617,-0.71039689228359));
#10745=CARTESIAN_POINT('Ctrl Pts',(95.6534634786373,2.10950140794812,-0.638451102172221));
#10746=CARTESIAN_POINT('Ctrl Pts',(95.6575220052697,2.13127641258827,-0.566504475734888));
#10747=CARTESIAN_POINT('Ctrl Pts',(95.6615805319021,2.14936551286382,-0.493446027386033));
#10748=CARTESIAN_POINT('Ctrl Pts',(95.6656390585345,2.16367253740287,-0.419686967737422));
#10749=CARTESIAN_POINT('Ctrl Pts',(95.6697017355196,2.17799419266959,-0.345852480195889));
#10750=CARTESIAN_POINT('Ctrl Pts',(95.6737644125047,2.18852595760925,-0.271316420384699));
#10751=CARTESIAN_POINT('Ctrl Pts',(95.6778270894898,2.19522301024608,-0.19649919919978));
#10752=CARTESIAN_POINT('Ctrl Pts',(95.6818918884669,2.20192356084541,-0.12164289995342));
#10753=CARTESIAN_POINT('Ctrl Pts',(95.6859566874439,2.20478539232686,-0.0465056244456972));
#10754=CARTESIAN_POINT('Ctrl Pts',(95.6900214864209,2.20381584438883,0.0284907707995336));
#10755=CARTESIAN_POINT('Ctrl Pts',(95.6940935466629,2.20284456447229,0.103621137909155));
#10756=CARTESIAN_POINT('Ctrl Pts',(95.698165606905,2.19802826484776,0.178609644888324));
#10757=CARTESIAN_POINT('Ctrl Pts',(95.702237667147,2.18942629103923,0.253038566440345));
#10758=CARTESIAN_POINT('Ctrl Pts',(95.7053758179458,2.18279714280103,0.310397536039677));
#10759=CARTESIAN_POINT('Ctrl Pts',(95.7085139687447,2.17392072501234,0.367424234420507));
#10760=CARTESIAN_POINT('Ctrl Pts',(95.7116521195436,2.16284466817774,0.423932708498817));
#10761=CARTESIAN_POINT('Ctrl Pts',(95.7157251844796,2.14846884572262,0.497276119668516));
#10762=CARTESIAN_POINT('Ctrl Pts',(95.7197982494156,2.13033039049547,0.570028900137833));
#10763=CARTESIAN_POINT('Ctrl Pts',(95.7238713143516,2.1084923097542,0.641775801746541));
#10764=CARTESIAN_POINT('Ctrl Pts',(95.7279383951566,2.08668631343496,0.713417293090574));
#10765=CARTESIAN_POINT('Ctrl Pts',(95.7320054759617,2.06119162111387,0.784055386697324));
#10766=CARTESIAN_POINT('Ctrl Pts',(95.7360725567667,2.03212227262231,0.853284869848483));
#10767=CARTESIAN_POINT('Ctrl Pts',(95.7401348791356,2.0030869349229,0.922433355327382));
#10768=CARTESIAN_POINT('Ctrl Pts',(95.7441972015045,1.97048543426028,0.990176066650771));
#10769=CARTESIAN_POINT('Ctrl Pts',(95.7482595238733,1.93448114142777,1.05612438351755));
#10770=CARTESIAN_POINT('Ctrl Pts',(95.7523192680126,1.89849969939927,1.12203084504027));
#10771=CARTESIAN_POINT('Ctrl Pts',(95.7563790121519,1.85911997899782,1.18614475401206));
#10772=CARTESIAN_POINT('Ctrl Pts',(95.7604387562913,1.81655227190928,1.24810009351063));
#10773=CARTESIAN_POINT('Ctrl Pts',(95.7644972357463,1.77399782543693,1.31003613279234));
#10774=CARTESIAN_POINT('Ctrl Pts',(95.7685557152014,1.72825763427084,1.36981454441949));
#10775=CARTESIAN_POINT('Ctrl Pts',(95.7726141946564,1.67958562172051,1.4270978029938));
#10776=CARTESIAN_POINT('Ctrl Pts',(95.7766727212888,1.63091304338781,1.48438172745096));
#10777=CARTESIAN_POINT('Ctrl Pts',(95.7807312479212,1.57930888652639,1.53917007857161));
#10778=CARTESIAN_POINT('Ctrl Pts',(95.7847897745536,1.52506666365048,1.59115922252363));
#10779=CARTESIAN_POINT('Ctrl Pts',(95.7888524515387,1.47076897129588,1.64320153189843));
#10780=CARTESIAN_POINT('Ctrl Pts',(95.7929151285238,1.41382817113154,1.6924385866597));
#10781=CARTESIAN_POINT('Ctrl Pts',(95.7969778055089,1.35457333061416,1.73860492694253));
#10782=CARTESIAN_POINT('Ctrl Pts',(95.8010426044859,1.29528754048039,1.78479538053847));
#10783=CARTESIAN_POINT('Ctrl Pts',(95.805107403463,1.2336856946048,1.82791165165345));
#10784=CARTESIAN_POINT('Ctrl Pts',(95.80917220244,1.17012633775186,1.86773133873676));
#10785=CARTESIAN_POINT('Ctrl Pts',(95.813244262682,1.1064534399011,1.90762215880864));
#10786=CARTESIAN_POINT('Ctrl Pts',(95.8173163229241,1.04081646405801,1.94420439935276));
#10787=CARTESIAN_POINT('Ctrl Pts',(95.8213883831661,0.973598660538437,1.97730160779729));
#10788=CARTESIAN_POINT('Ctrl Pts',(95.824526533965,0.921796970170994,2.00280811431936));
#10789=CARTESIAN_POINT('Ctrl Pts',(95.8276646847639,0.869056935062801,2.0262457724316));
#10790=CARTESIAN_POINT('Ctrl Pts',(95.8308028355628,0.815560654889221,2.04755386209903));
#10791=CARTESIAN_POINT('Ctrl Pts',(95.8353960033341,0.737260596757818,2.07874153821811));
#10792=CARTESIAN_POINT('Ctrl Pts',(95.8399891711054,0.657087046343997,2.10546688559112));
#10793=CARTESIAN_POINT('Ctrl Pts',(95.8445823388767,0.575530641081532,2.12752919631583));
#10794=CARTESIAN_POINT('Ctrl Pts',(95.8491582578205,0.494280506444697,2.14950865594274));
#10795=CARTESIAN_POINT('Ctrl Pts',(95.8537341767643,0.411658102933076,2.16685989473513));
#10796=CARTESIAN_POINT('Ctrl Pts',(95.8583100957081,0.328170611828205,2.17943112979794));
#10797=CARTESIAN_POINT('Ctrl Pts',(95.8628571209176,0.245210285958407,2.19192298628559));
#10798=CARTESIAN_POINT('Ctrl Pts',(95.8674041461271,0.161395999516733,2.19969489573444));
#10799=CARTESIAN_POINT('Ctrl Pts',(95.8719511713365,0.077243792355056,2.20264599891644));
#10800=CARTESIAN_POINT('Ctrl Pts',(95.8733169164828,0.0519678233012755,
2.20353239269289));
#10801=CARTESIAN_POINT('Ctrl Pts',(95.8746826616292,0.0266614814832344,
2.2039842087331));
#10802=CARTESIAN_POINT('Ctrl Pts',(95.8760484067755,0.00133902696002845,
2.20399959324107));
#10803=CARTESIAN_POINT('',(96.6260484068518,-0.0017560042200646,2.20399930046477));
#10804=CARTESIAN_POINT('Ctrl Pts',(95.8760484068025,0.00133902645877407,
2.20399959324137));
#10805=CARTESIAN_POINT('Ctrl Pts',(95.8801415572499,-0.0745525967635283,
2.20404570073241));
#10806=CARTESIAN_POINT('Ctrl Pts',(95.8842347076972,-0.150456680726987,
2.20016763868404));
#10807=CARTESIAN_POINT('Ctrl Pts',(95.8883278581446,-0.225943957588798,
2.19238804230207));
#10808=CARTESIAN_POINT('Ctrl Pts',(95.8924217124816,-0.301444215823037,
2.18460710808091));
#10809=CARTESIAN_POINT('Ctrl Pts',(95.8965155668186,-0.376527061147336,
2.17292335529049));
#10810=CARTESIAN_POINT('Ctrl Pts',(95.9006094211556,-0.450769289729901,
2.15741119108908));
#10811=CARTESIAN_POINT('Ctrl Pts',(95.9047214320244,-0.525340787817131,
2.14183022934858));
#10812=CARTESIAN_POINT('Ctrl Pts',(95.9088334428933,-0.599063731269043,
2.12238691207033));
#10813=CARTESIAN_POINT('Ctrl Pts',(95.9129454537622,-0.671522599166809,
2.0992078026742));
#10814=CARTESIAN_POINT('Ctrl Pts',(95.9170471156906,-0.743799105555967,
2.07608702951048));
#10815=CARTESIAN_POINT('Ctrl Pts',(95.9211487776191,-0.814817469942279,
2.04924945607877));
#10816=CARTESIAN_POINT('Ctrl Pts',(95.9252504395475,-0.884185175174658,
2.01886913295572));
#10817=CARTESIAN_POINT('Ctrl Pts',(95.9293676248866,-0.953815413836089,
1.98837383052956));
#10818=CARTESIAN_POINT('Ctrl Pts',(95.9334848102257,-1.02178205961179,1.95430913518859));
#10819=CARTESIAN_POINT('Ctrl Pts',(95.9376019955647,-1.08771450162772,1.91689675333565));
#10820=CARTESIAN_POINT('Ctrl Pts',(95.9417191809038,-1.15364694364365,1.87948437148271));
#10821=CARTESIAN_POINT('Ctrl Pts',(95.9458363662428,-1.21754482386606,1.83872461058378));
#10822=CARTESIAN_POINT('Ctrl Pts',(95.9499535515819,-1.27906965800229,1.79488072305039));
#10823=CARTESIAN_POINT('Ctrl Pts',(95.9540266165179,-1.33993518237773,1.75150667348419));
#10824=CARTESIAN_POINT('Ctrl Pts',(95.9580996814539,-1.398709319395,1.70494948884079));
#10825=CARTESIAN_POINT('Ctrl Pts',(95.9621727463899,-1.45503987674905,1.65543799553777));
#10826=CARTESIAN_POINT('Ctrl Pts',(95.9662398271949,-1.51128767347052,1.60599924432533));
#10827=CARTESIAN_POINT('Ctrl Pts',(95.970306908,-1.56509866269076,1.55361511462868));
#10828=CARTESIAN_POINT('Ctrl Pts',(95.9743739888051,-1.61615086168616,1.49855676978588));
#10829=CARTESIAN_POINT('Ctrl Pts',(95.9784363111739,-1.66714333021566,1.44356284255199));
#10830=CARTESIAN_POINT('Ctrl Pts',(95.9824986335428,-1.71538309831979,1.38590126473668));
#10831=CARTESIAN_POINT('Ctrl Pts',(95.9865609559117,-1.76058366238125,1.32588127966128));
#10832=CARTESIAN_POINT('Ctrl Pts',(95.990620700051,-1.80575553905165,1.26589938740218));
#10833=CARTESIAN_POINT('Ctrl Pts',(95.9946804441903,-1.84789175284692,1.20356243857123));
#10834=CARTESIAN_POINT('Ctrl Pts',(95.9987401883296,-1.88674575898031,1.1392130797045));
#10835=CARTESIAN_POINT('Ctrl Pts',(96.0027986677846,-1.925587661383,1.0748837668353));
#10836=CARTESIAN_POINT('Ctrl Pts',(96.0068571472397,-1.96114913955829,1.00854369708425));
#10837=CARTESIAN_POINT('Ctrl Pts',(96.0109156266947,-1.99322761242658,0.940563493369933));
#10838=CARTESIAN_POINT('Ctrl Pts',(96.0149741533271,-2.02530645818755,0.872582499427198));
#10839=CARTESIAN_POINT('Ctrl Pts',(96.0190326799595,-2.05390201611521,0.802961766231307));
#10840=CARTESIAN_POINT('Ctrl Pts',(96.0230912065919,-2.07885891820595,0.732093981805324));
#10841=CARTESIAN_POINT('Ctrl Pts',(96.027153883577,-2.10384134186037,0.661153726178143));
#10842=CARTESIAN_POINT('Ctrl Pts',(96.0312165605621,-2.1251775201404,0.588964324038188));
#10843=CARTESIAN_POINT('Ctrl Pts',(96.0352792375472,-2.14276153291415,0.515935086094572));
#10844=CARTESIAN_POINT('Ctrl Pts',(96.0393440365243,-2.1603547300591,0.442867703977705));
#10845=CARTESIAN_POINT('Ctrl Pts',(96.0434088355013,-2.17419177098629,0.368960082256197));
#10846=CARTESIAN_POINT('Ctrl Pts',(96.0474736344784,-2.18421812285109,0.294630602295251));
#10847=CARTESIAN_POINT('Ctrl Pts',(96.0515456947204,-2.19426238556412,0.220168341832275));
#10848=CARTESIAN_POINT('Ctrl Pts',(96.0556177549624,-2.20048232252395,0.145283194404663));
#10849=CARTESIAN_POINT('Ctrl Pts',(96.0596898152044,-2.20287545090114,0.0703970725036641));
#10850=CARTESIAN_POINT('Ctrl Pts',(96.0628279660033,-2.20471972561281,0.0126857594823805));
#10851=CARTESIAN_POINT('Ctrl Pts',(96.0659661168022,-2.20429229956221,-0.0450260454446914));
#10852=CARTESIAN_POINT('Ctrl Pts',(96.069104267601,-2.2016130511633,-0.102547418043673));
#10853=CARTESIAN_POINT('Ctrl Pts',(96.073177332537,-2.19813560428206,-0.177205489251421));
#10854=CARTESIAN_POINT('Ctrl Pts',(96.077250397473,-2.19084959419916,-0.251830449426423));
#10855=CARTESIAN_POINT('Ctrl Pts',(96.081323462409,-2.17975652317247,-0.326002300125415));
#10856=CARTESIAN_POINT('Ctrl Pts',(96.0853905432141,-2.16867975004198,-0.400065177833923));
#10857=CARTESIAN_POINT('Ctrl Pts',(96.0894576240191,-2.15380709102484,-0.473675799477012));
#10858=CARTESIAN_POINT('Ctrl Pts',(96.0935247048242,-2.13519200048681,-0.546416618577013));
#10859=CARTESIAN_POINT('Ctrl Pts',(96.097587027193,-2.11659868938336,-0.61907233178359));
#10860=CARTESIAN_POINT('Ctrl Pts',(96.1016493495619,-2.09427176381602,-0.69085980407235));
#10861=CARTESIAN_POINT('Ctrl Pts',(96.1057116719308,-2.06831590746407,-0.761370676432365));
#10862=CARTESIAN_POINT('Ctrl Pts',(96.1097714160701,-2.04237652448626,-0.831836797736386));
#10863=CARTESIAN_POINT('Ctrl Pts',(96.1138311602094,-2.0128129456352,-0.901027479970799));
#10864=CARTESIAN_POINT('Ctrl Pts',(96.1178909043487,-1.97977958031341,-0.968549850742891));
#10865=CARTESIAN_POINT('Ctrl Pts',(96.1219493838038,-1.94675650548668,-1.03605118706644));
#10866=CARTESIAN_POINT('Ctrl Pts',(96.1260078632588,-1.91026599995695,-1.10188481518128));
#10867=CARTESIAN_POINT('Ctrl Pts',(96.1300663427139,-1.87050980755325,-1.16567965575757));
#10868=CARTESIAN_POINT('Ctrl Pts',(96.1341248693463,-1.8307531530082,-1.22947523790977));
#10869=CARTESIAN_POINT('Ctrl Pts',(96.1381833959787,-1.78773099026223,-1.29123158119967));
#10870=CARTESIAN_POINT('Ctrl Pts',(96.142241922611,-1.74168918975071,-1.35060533328783));
#10871=CARTESIAN_POINT('Ctrl Pts',(96.1463045995961,-1.69560030572121,-1.41003980248724));
#10872=CARTESIAN_POINT('Ctrl Pts',(96.1503672765812,-1.64648591068597,-1.46708643678975));
#10873=CARTESIAN_POINT('Ctrl Pts',(96.1544299535663,-1.59463263822371,-1.5214344379932));
#10874=CARTESIAN_POINT('Ctrl Pts',(96.1584947525434,-1.54275228208562,-1.57581082590354));
#10875=CARTESIAN_POINT('Ctrl Pts',(96.1625595515204,-1.48813054687872,-1.62748544533259));
#10876=CARTESIAN_POINT('Ctrl Pts',(96.1666243504975,-1.43108953270281,-1.67618577412782));
#10877=CARTESIAN_POINT('Ctrl Pts',(96.1706964107395,-1.37394662174913,-1.72497310008906));
#10878=CARTESIAN_POINT('Ctrl Pts',(96.1747684709815,-1.31437617854984,-1.77077523124125));
#10879=CARTESIAN_POINT('Ctrl Pts',(96.1788405312235,-1.25273147286246,-1.81336147993164));
#10880=CARTESIAN_POINT('Ctrl Pts',(96.1819786820224,-1.20522471439048,-1.84618075627017));
#10881=CARTESIAN_POINT('Ctrl Pts',(96.1851168328213,-1.15648668836683,-1.87709094779876));
#10882=CARTESIAN_POINT('Ctrl Pts',(96.1882549836202,-1.10668863603713,-1.90600531553988));
#10883=CARTESIAN_POINT('Ctrl Pts',(96.1923280485562,-1.04205480744733,-1.94353381717664));
#10884=CARTESIAN_POINT('Ctrl Pts',(96.1964011134922,-0.975385250761897,
-1.97784330326168));
#10885=CARTESIAN_POINT('Ctrl Pts',(96.2004741784282,-0.907033786194218,
-2.00870747265553));
#10886=CARTESIAN_POINT('Ctrl Pts',(96.2045412592333,-0.838782743328431,
-2.03952629653357));
#10887=CARTESIAN_POINT('Ctrl Pts',(96.2086083400383,-0.768855130169087,
-2.06690965868656));
#10888=CARTESIAN_POINT('Ctrl Pts',(96.2126754208434,-0.697630854785237,
-2.09067625194616));
#10889=CARTESIAN_POINT('Ctrl Pts',(96.2167377432123,-0.626489910957011,
-2.11441503857412));
#10890=CARTESIAN_POINT('Ctrl Pts',(96.2208000655811,-0.554055769629776,
-2.13454531311469));
#10891=CARTESIAN_POINT('Ctrl Pts',(96.22486238795,-0.480728373953735,-2.15093380429891));
#10892=CARTESIAN_POINT('Ctrl Pts',(96.2289221320893,-0.407447516893365,
-2.16731189421789));
#10893=CARTESIAN_POINT('Ctrl Pts',(96.2329818762286,-0.333274995260967,
-2.1799528094234));
#10894=CARTESIAN_POINT('Ctrl Pts',(96.2370416203679,-0.258624678211475,
-2.18877346379657));
#10895=CARTESIAN_POINT('Ctrl Pts',(96.241100099823,-0.183997616095518,-2.19759137037522));
#10896=CARTESIAN_POINT('Ctrl Pts',(96.245158579278,-0.108893527934604,-2.20259132298585));
#10897=CARTESIAN_POINT('Ctrl Pts',(96.2492170587331,-0.0337336127045116,
-2.20374182774977));
#10898=CARTESIAN_POINT('Ctrl Pts',(96.2532755853654,0.0414271762135432,
-2.2048923458876));
#10899=CARTESIAN_POINT('Ctrl Pts',(96.2573341119978,0.116643316057064,-2.20219332181591));
#10900=CARTESIAN_POINT('Ctrl Pts',(96.2613926386302,0.191493003523942,-2.19566537286568));
#10901=CARTESIAN_POINT('Ctrl Pts',(96.2654553156153,0.266419234187636,-2.18913074826858));
#10902=CARTESIAN_POINT('Ctrl Pts',(96.2695179926004,0.340977787421396,-2.17875942122692));
#10903=CARTESIAN_POINT('Ctrl Pts',(96.2735806695855,0.414752135179091,-2.16462390875745));
#10904=CARTESIAN_POINT('Ctrl Pts',(96.2776454685626,0.48856501629114,-2.15048101311582));
#10905=CARTESIAN_POINT('Ctrl Pts',(96.2817102675396,0.561592412097398,-2.13257013061648));
#10906=CARTESIAN_POINT('Ctrl Pts',(96.2857750665166,0.633430748860622,-2.11101432643122));
#10907=CARTESIAN_POINT('Ctrl Pts',(96.2898471267586,0.705397416004021,-2.08942001544485));
#10908=CARTESIAN_POINT('Ctrl Pts',(96.2939191870007,0.776170331002954,-2.06416793783538));
#10909=CARTESIAN_POINT('Ctrl Pts',(96.2979912472427,0.84536419341451,-2.03543002348217));
#10910=CARTESIAN_POINT('Ctrl Pts',(96.3011293980416,0.898688742094799,-2.01328302576462));
#10911=CARTESIAN_POINT('Ctrl Pts',(96.3042675488404,0.951075842084046,-1.9890667734598));
#10912=CARTESIAN_POINT('Ctrl Pts',(96.3074056996393,1.00235980775178,-1.96287819688432));
#10913=CARTESIAN_POINT('Ctrl Pts',(96.3114787645753,1.06892223120658,-1.92888755086076));
#10914=CARTESIAN_POINT('Ctrl Pts',(96.3155518295113,1.1338820900052,-1.89144175845474));
#10915=CARTESIAN_POINT('Ctrl Pts',(96.3196248944473,1.19685747229546,-1.85071558890353));
#10916=CARTESIAN_POINT('Ctrl Pts',(96.3236919752523,1.25974033140259,-1.81004925407989));
#10917=CARTESIAN_POINT('Ctrl Pts',(96.3277590560574,1.32064410502822,-1.76611236794642));
#10918=CARTESIAN_POINT('Ctrl Pts',(96.3318261368624,1.37921056355657,-1.7191260050892));
#10919=CARTESIAN_POINT('Ctrl Pts',(96.3358884592313,1.4377085000247,-1.67219461571794));
#10920=CARTESIAN_POINT('Ctrl Pts',(96.3399507816002,1.49387418393377,-1.62222113541162));
#10921=CARTESIAN_POINT('Ctrl Pts',(96.3440131039691,1.54737890414502,-1.56946950496242));
#10922=CARTESIAN_POINT('Ctrl Pts',(96.3480728481084,1.60084966657576,-1.51675135433109));
#10923=CARTESIAN_POINT('Ctrl Pts',(96.3521325922477,1.65166247747263,-1.46125888681238));
#10924=CARTESIAN_POINT('Ctrl Pts',(96.356192336387,1.69952326062962,-1.40329493926931));
#10925=CARTESIAN_POINT('Ctrl Pts',(96.3602508158421,1.74736913428081,-1.3453490485518));
#10926=CARTESIAN_POINT('Ctrl Pts',(96.3643092952971,1.79226450223659,-1.28493357436921));
#10927=CARTESIAN_POINT('Ctrl Pts',(96.3683677747522,1.83395467982266,-1.22238546799141));
#10928=CARTESIAN_POINT('Ctrl Pts',(96.3724263013846,1.87564534203156,-1.15983663453009));
#10929=CARTESIAN_POINT('Ctrl Pts',(96.376484828017,1.9141304765749,-1.09515551794187));
#10930=CARTESIAN_POINT('Ctrl Pts',(96.3805433546494,1.94919887051189,-1.02870781235255));
#10931=CARTESIAN_POINT('Ctrl Pts',(96.3846060316345,1.98430312628168,-0.962192155647132));
#10932=CARTESIAN_POINT('Ctrl Pts',(96.3886687086196,2.01598344068688,-0.893906725545878));
#10933=CARTESIAN_POINT('Ctrl Pts',(96.3927313856047,2.04407508041402,-0.824240902667667));
#10934=CARTESIAN_POINT('Ctrl Pts',(96.3967961845817,2.07218139279014,-0.75453869237403));
#10935=CARTESIAN_POINT('Ctrl Pts',(96.4008609835588,2.09669514197037,-0.683455105300154));
#10936=CARTESIAN_POINT('Ctrl Pts',(96.4049257825358,2.11750109898325,-0.611396022071397));
#10937=CARTESIAN_POINT('Ctrl Pts',(96.4089978427778,2.13834422328721,-0.539208214125991));
#10938=CARTESIAN_POINT('Ctrl Pts',(96.4130699030198,2.15546621650982,-0.466041894899636));
#10939=CARTESIAN_POINT('Ctrl Pts',(96.4171419632619,2.16880282102937,-0.392314062321301));
#10940=CARTESIAN_POINT('Ctrl Pts',(96.4202801140607,2.1790807328577,-0.335495389965608));
#10941=CARTESIAN_POINT('Ctrl Pts',(96.4234182648596,2.18711151924388,-0.278343473191536));
#10942=CARTESIAN_POINT('Ctrl Pts',(96.4265564156584,2.19288687768179,-0.221050088647333));
#10943=CARTESIAN_POINT('Ctrl Pts',(96.4306294805944,2.20038282400623,-0.146687927422888));
#10944=CARTESIAN_POINT('Ctrl Pts',(96.4347025455304,2.20410643737698,-0.0718006432719025));
#10945=CARTESIAN_POINT('Ctrl Pts',(96.4387756104664,2.20399768264422,0.00319607554513029));
#10946=CARTESIAN_POINT('Ctrl Pts',(96.4428426912715,2.20388908769349,0.0780826094788758));
#10947=CARTESIAN_POINT('Ctrl Pts',(96.4469097720766,2.19995930416598,0.153077785366209));
#10948=CARTESIAN_POINT('Ctrl Pts',(96.4509768528816,2.19220004781124,0.227760730540615));
#10949=CARTESIAN_POINT('Ctrl Pts',(96.4550391752505,2.18444986969419,0.302356297557017));
#10950=CARTESIAN_POINT('Ctrl Pts',(96.4591014976194,2.17287916944965,0.376639887122612));
#10951=CARTESIAN_POINT('Ctrl Pts',(96.4631638199882,2.15753168534196,0.450192210889408));
#10952=CARTESIAN_POINT('Ctrl Pts',(96.4672235641276,2.14219394180472,0.523697853285732));
#10953=CARTESIAN_POINT('Ctrl Pts',(96.4712833082668,2.12308426828563,0.596472684653092));
#10954=CARTESIAN_POINT('Ctrl Pts',(96.4753430524062,2.10029786088887,0.668105452414248));
#10955=CARTESIAN_POINT('Ctrl Pts',(96.4794015318612,2.07751855187313,0.739715905263258));
#10956=CARTESIAN_POINT('Ctrl Pts',(96.4834600113163,2.05106492770177,0.810184546180891));
#10957=CARTESIAN_POINT('Ctrl Pts',(96.4875184907713,2.02108220058087,0.879114747058197));
#10958=CARTESIAN_POINT('Ctrl Pts',(96.4915770174037,1.99109912492907,0.948045749207003));
#10959=CARTESIAN_POINT('Ctrl Pts',(96.4956355440361,1.95758705696382,1.0154378386879));
#10960=CARTESIAN_POINT('Ctrl Pts',(96.4996940706685,1.92073892097277,1.08091535166282));
#10961=CARTESIAN_POINT('Ctrl Pts',(96.5037567476536,1.88385310313939,1.14645982361014));
#10962=CARTESIAN_POINT('Ctrl Pts',(96.5078194246387,1.84362463929627,1.21008539222633));
#10963=CARTESIAN_POINT('Ctrl Pts',(96.5118821016238,1.80029154570757,1.27144262570273));
#10964=CARTESIAN_POINT('Ctrl Pts',(96.5159469006008,1.75693581864943,1.33283190690418));
#10965=CARTESIAN_POINT('Ctrl Pts',(96.5200116995779,1.71047252791787,1.39195011784231));
#10966=CARTESIAN_POINT('Ctrl Pts',(96.5240764985549,1.66118038040572,1.44848049477897));
#10967=CARTESIAN_POINT('Ctrl Pts',(96.5281485587969,1.61180017851593,1.50511185630261));
#10968=CARTESIAN_POINT('Ctrl Pts',(96.532220619039,1.55958135835212,1.55914580620202));
#10969=CARTESIAN_POINT('Ctrl Pts',(96.536292679281,1.50483958816004,1.61030239828));
#10970=CARTESIAN_POINT('Ctrl Pts',(96.5394308300799,1.46265260671785,1.64972644673636));
#10971=CARTESIAN_POINT('Ctrl Pts',(96.5425689808787,1.41896799657714,1.68744235793924));
#10972=CARTESIAN_POINT('Ctrl Pts',(96.5457071316776,1.37394244643187,1.72333924515541));
#10973=CARTESIAN_POINT('Ctrl Pts',(96.549771968387,1.31562099509928,1.76983636854456));
#10974=CARTESIAN_POINT('Ctrl Pts',(96.5538368050965,1.25481867372989,1.8134635003033));
#10975=CARTESIAN_POINT('Ctrl Pts',(96.5579016418059,1.19184989068572,1.85394439994096));
#10976=CARTESIAN_POINT('Ctrl Pts',(96.5619606890479,1.12897079284792,1.89436764342484));
#10977=CARTESIAN_POINT('Ctrl Pts',(96.5660197362898,1.06393175466375,1.93165328948619));
#10978=CARTESIAN_POINT('Ctrl Pts',(96.5700787835318,0.997079888480288,1.96556549012953));
#10979=CARTESIAN_POINT('Ctrl Pts',(96.574133372363,0.930301451617452,1.99944044200188));
#10980=CARTESIAN_POINT('Ctrl Pts',(96.5781879611942,0.861714563893496,2.02994908790959));
#10981=CARTESIAN_POINT('Ctrl Pts',(96.5822425500254,0.791693557190234,2.05689992744019));
#10982=CARTESIAN_POINT('Ctrl Pts',(96.5862942938241,0.721721682975405,2.08383185604858));
#10983=CARTESIAN_POINT('Ctrl Pts',(96.5903460376228,0.650318132728327,2.10721076118897));
#10984=CARTESIAN_POINT('Ctrl Pts',(96.5943977814215,0.577878578333352,2.12689265095901));
#10985=CARTESIAN_POINT('Ctrl Pts',(96.5984478135306,0.505469626571626,2.14656622596704));
#10986=CARTESIAN_POINT('Ctrl Pts',(96.6024978456397,0.432026002467835,2.16254576459369));
#10987=CARTESIAN_POINT('Ctrl Pts',(96.6065478777489,0.357958330807542,2.17473718720343));
#10988=CARTESIAN_POINT('Ctrl Pts',(96.6105987786785,0.283874770010601,2.18693122514015));
#10989=CARTESIAN_POINT('Ctrl Pts',(96.6146496796082,0.209167366512248,2.19533544172223));
#10990=CARTESIAN_POINT('Ctrl Pts',(96.6187005805378,0.134255495671819,2.1999071484683));
#10991=CARTESIAN_POINT('Ctrl Pts',(96.6211498559594,0.0889619159919616,
2.20267131603551));
#10992=CARTESIAN_POINT('Ctrl Pts',(96.623599131381,0.043593721674534,2.20403543217708));
#10993=CARTESIAN_POINT('Ctrl Pts',(96.6260484068025,-0.00175600330752527,
2.20399930046549));
#10994=CARTESIAN_POINT('',(97.3760484067751,-0.000421831323932275,2.20399995963211));
#10995=CARTESIAN_POINT('Ctrl Pts',(96.6260484068518,-0.00175600422006416,
2.20399930046477));
#10996=CARTESIAN_POINT('Ctrl Pts',(96.6308098313547,-0.0899164821416865,
2.20392905989289));
#10997=CARTESIAN_POINT('Ctrl Pts',(96.6355712558577,-0.177854000831902,
2.19856523823089));
#10998=CARTESIAN_POINT('Ctrl Pts',(96.6403326803606,-0.264996210083368,
2.18801119938666));
#10999=CARTESIAN_POINT('Ctrl Pts',(96.6451473637233,-0.353113147528027,
2.17733910846065));
#11000=CARTESIAN_POINT('Ctrl Pts',(96.649962047086,-0.440416778753674,2.1613601370602));
#11001=CARTESIAN_POINT('Ctrl Pts',(96.6547767304487,-0.526336028431881,
2.14023045141745));
#11002=CARTESIAN_POINT('Ctrl Pts',(96.6581371028647,-0.586302729224979,
2.12548314459697));
#11003=CARTESIAN_POINT('Ctrl Pts',(96.6614974752808,-0.645595498506252,
2.10822782962978));
#11004=CARTESIAN_POINT('Ctrl Pts',(96.6648578476968,-0.704026432666069,
2.08853124997149));
#11005=CARTESIAN_POINT('Ctrl Pts',(96.6689309126328,-0.774849829492498,
2.06465727469931));
#11006=CARTESIAN_POINT('Ctrl Pts',(96.6730039775688,-0.844594055879215,
2.03713067829103));
#11007=CARTESIAN_POINT('Ctrl Pts',(96.6770770425048,-0.912855719265293,
2.00606840257371));
#11008=CARTESIAN_POINT('Ctrl Pts',(96.6811441233099,-0.981017092884918,
1.97505176342929));
#11009=CARTESIAN_POINT('Ctrl Pts',(96.685211204115,-1.04769979709705,1.94050995450216));
#11010=CARTESIAN_POINT('Ctrl Pts',(96.6892782849201,-1.11251708334427,1.9026091924689));
#11011=CARTESIAN_POINT('Ctrl Pts',(96.693340607289,-1.17725853413712,1.86475277387667));
#11012=CARTESIAN_POINT('Ctrl Pts',(96.6974029296579,-1.2401384930298,1.82354544986018));
#11013=CARTESIAN_POINT('Ctrl Pts',(96.7014652520268,-1.30079313252182,1.77920016478868));
#11014=CARTESIAN_POINT('Ctrl Pts',(96.7055249961661,-1.36140927640207,1.73488302428934));
#11015=CARTESIAN_POINT('Ctrl Pts',(96.7095847403054,-1.41980251906175,1.68743215586438));
#11016=CARTESIAN_POINT('Ctrl Pts',(96.7136444844448,-1.47563759686912,1.63710405371996));
#11017=CARTESIAN_POINT('Ctrl Pts',(96.7177029638998,-1.53145528103266,1.58679162969614));
#11018=CARTESIAN_POINT('Ctrl Pts',(96.7217614433549,-1.58471602816388,1.53360407100371));
#11019=CARTESIAN_POINT('Ctrl Pts',(96.72581992281,-1.63511854420886,1.47783738834294));
#11020=CARTESIAN_POINT('Ctrl Pts',(96.7298784494424,-1.68552164615227,1.4220700574286));
#11021=CARTESIAN_POINT('Ctrl Pts',(96.7339369760748,-1.73306613222038,1.3637238984421));
#11022=CARTESIAN_POINT('Ctrl Pts',(96.7379955027072,-1.77748950095122,1.30312972263247));
#11023=CARTESIAN_POINT('Ctrl Pts',(96.7420581796923,-1.82195829815037,1.24247358167534));
#11024=CARTESIAN_POINT('Ctrl Pts',(96.7461208566774,-1.8632993213725,1.17956521908401));
#11025=CARTESIAN_POINT('Ctrl Pts',(96.7501835336626,-1.90129257785128,1.11476568542794));
#11026=CARTESIAN_POINT('Ctrl Pts',(96.7542483326396,-1.93930567872936,1.04993230608611));
#11027=CARTESIAN_POINT('Ctrl Pts',(96.7583131316167,-1.97396731042543,0.983206212701497));
#11028=CARTESIAN_POINT('Ctrl Pts',(96.7623779305937,-2.00510403363176,0.914972029252061));
#11029=CARTESIAN_POINT('Ctrl Pts',(96.7664499908358,-2.03629637877627,0.846615953800434));
#11030=CARTESIAN_POINT('Ctrl Pts',(96.7705220510778,-2.06395106204914,0.776746851801219));
#11031=CARTESIAN_POINT('Ctrl Pts',(96.7745941113198,-2.08794343724145,0.705767810884249));
#11032=CARTESIAN_POINT('Ctrl Pts',(96.7777322621185,-2.10643326472366,0.651067506688116));
#11033=CARTESIAN_POINT('Ctrl Pts',(96.7808704129172,-2.12274901846192,0.595708394515493));
#11034=CARTESIAN_POINT('Ctrl Pts',(96.7840085637159,-2.13685439413681,0.539878966304667));
#11035=CARTESIAN_POINT('Ctrl Pts',(96.7880816286519,-2.15516202648322,0.4674169015322));
#11036=CARTESIAN_POINT('Ctrl Pts',(96.7921546935879,-2.16981493522022,0.393882808150005));
#11037=CARTESIAN_POINT('Ctrl Pts',(96.7962277585238,-2.18069284290564,0.319679096751906));
#11038=CARTESIAN_POINT('Ctrl Pts',(96.8002948393289,-2.19155476881201,0.245584405153781));
#11039=CARTESIAN_POINT('Ctrl Pts',(96.8043619201339,-2.19865263649152,0.170822517274372));
#11040=CARTESIAN_POINT('Ctrl Pts',(96.8084290009389,-2.20191660179042,0.0958085526439572));
#11041=CARTESIAN_POINT('Ctrl Pts',(96.8124913233078,-2.20517674828873,0.0208823534603541));
#11042=CARTESIAN_POINT('Ctrl Pts',(96.8165536456766,-2.20461188365891,-0.0542948619096966));
#11043=CARTESIAN_POINT('Ctrl Pts',(96.8206159680455,-2.20020385720147,-0.129301920928357));
#11044=CARTESIAN_POINT('Ctrl Pts',(96.8246757121848,-2.19579862838122,-0.20426137530135));
#11045=CARTESIAN_POINT('Ctrl Pts',(96.8287354563241,-2.1875551058737,-0.279050412192913));
#11046=CARTESIAN_POINT('Ctrl Pts',(96.8327952004633,-2.17550721885559,-0.35324827063585));
#11047=CARTESIAN_POINT('Ctrl Pts',(96.8368536799184,-2.16346308497376,-0.427423015094262));
#11048=CARTESIAN_POINT('Ctrl Pts',(96.8409121593734,-2.14761701607951,-0.501006475770795));
#11049=CARTESIAN_POINT('Ctrl Pts',(96.8449706388284,-2.1280545601486,-0.573585032083948));
#11050=CARTESIAN_POINT('Ctrl Pts',(96.8490291654608,-2.10849187681611,-0.646164432078399));
#11051=CARTESIAN_POINT('Ctrl Pts',(96.8530876920932,-2.08521284665938,-0.717738443973867));
#11052=CARTESIAN_POINT('Ctrl Pts',(96.8571462187255,-2.05835328593649,-0.787907196486008));
#11053=CARTESIAN_POINT('Ctrl Pts',(96.8612088957106,-2.03146625794269,-0.858147705351686));
#11054=CARTESIAN_POINT('Ctrl Pts',(96.8652715726957,-2.00099155855932,-0.926979638219817));
#11055=CARTESIAN_POINT('Ctrl Pts',(96.8693342496808,-1.96711345210214,-0.994022467834));
#11056=CARTESIAN_POINT('Ctrl Pts',(96.8733990486578,-1.933217650645,-1.06110031483822));
#11057=CARTESIAN_POINT('Ctrl Pts',(96.8774638476348,-1.89591513919266,-1.12638678272741));
#11058=CARTESIAN_POINT('Ctrl Pts',(96.8815286466119,-1.85543521899374,-1.18952769960084));
#11059=CARTESIAN_POINT('Ctrl Pts',(96.8856007068539,-1.81488298638082,-1.25278140998025));
#11060=CARTESIAN_POINT('Ctrl Pts',(96.8896727670959,-1.77114228589202,-1.31388152488797));
#11061=CARTESIAN_POINT('Ctrl Pts',(96.8937448273379,-1.72448437447102,-1.37250487875464));
#11062=CARTESIAN_POINT('Ctrl Pts',(96.8968829781369,-1.68852725367541,-1.41768321940962));
#11063=CARTESIAN_POINT('Ctrl Pts',(96.900021128936,-1.65083845080548,-1.46139121935922));
#11064=CARTESIAN_POINT('Ctrl Pts',(96.903159279735,-1.61155672181826,-1.50349623623154));
#11065=CARTESIAN_POINT('Ctrl Pts',(96.907232344671,-1.5605722270612,-1.55814512942743));
#11066=CARTESIAN_POINT('Ctrl Pts',(96.911305409607,-1.50670649418841,-1.6103030957032));
#11067=CARTESIAN_POINT('Ctrl Pts',(96.9153784745429,-1.45023257818622,-1.65965100824461));
#11068=CARTESIAN_POINT('Ctrl Pts',(96.9194455553479,-1.39384163343858,-1.70892641902764));
#11069=CARTESIAN_POINT('Ctrl Pts',(96.923512636153,-1.33485047006253,-1.75539966131159));
#11070=CARTESIAN_POINT('Ctrl Pts',(96.927579716958,-1.2735701506229,-1.79878711120643));
#11071=CARTESIAN_POINT('Ctrl Pts',(96.9316420393268,-1.21236152842848,-1.8421237983007));
#11072=CARTESIAN_POINT('Ctrl Pts',(96.9357043616957,-1.14886945903196,-1.88238159141643));
#11073=CARTESIAN_POINT('Ctrl Pts',(96.9397666840645,-1.08343810109065,-1.91931703506875));
#11074=CARTESIAN_POINT('Ctrl Pts',(96.9438264282038,-1.01804827039561,-1.95622903694463));
#11075=CARTESIAN_POINT('Ctrl Pts',(96.9478861723431,-0.950722008292447,
-1.98982263951525));
#11076=CARTESIAN_POINT('Ctrl Pts',(96.9519459164823,-0.881831345461783,
-2.01989838312749));
#11077=CARTESIAN_POINT('Ctrl Pts',(96.9560043959374,-0.812962143327503,
-2.04996475759774));
#11078=CARTESIAN_POINT('Ctrl Pts',(96.9600628753924,-0.742529945349692,
-2.07651525801702));
#11079=CARTESIAN_POINT('Ctrl Pts',(96.9641213548474,-0.670928748881124,
-2.09939767884144));
#11080=CARTESIAN_POINT('Ctrl Pts',(96.9681798814798,-0.599326720092509,
-2.12228036565998));
#11081=CARTESIAN_POINT('Ctrl Pts',(96.9722384081121,-0.526556121178033,
-2.14149474458408));
#11082=CARTESIAN_POINT('Ctrl Pts',(96.9762969347445,-0.45302662967315,-2.15693830992149));
#11083=CARTESIAN_POINT('Ctrl Pts',(96.9803596117295,-0.379421945037426,
-2.17239766824217));
#11084=CARTESIAN_POINT('Ctrl Pts',(96.9844222887146,-0.305057286361621,
-2.18407841414576));
#11085=CARTESIAN_POINT('Ctrl Pts',(96.9884849656997,-0.230352322789945,
-2.19192924324333));
#11086=CARTESIAN_POINT('Ctrl Pts',(96.9925497646767,-0.155608339790519,
-2.19978417293669));
#11087=CARTESIAN_POINT('Ctrl Pts',(96.9966145636537,-0.080524175152663,
-2.20380517662948));
#11088=CARTESIAN_POINT('Ctrl Pts',(97.0006793626307,-0.00552174843155068,
-2.20399308308676));
#11089=CARTESIAN_POINT('Ctrl Pts',(97.0047514228727,0.0696146609284717,
-2.20418132521588));
#11090=CARTESIAN_POINT('Ctrl Pts',(97.0088234831146,0.144668563116419,-2.20052281632401));
#11091=CARTESIAN_POINT('Ctrl Pts',(97.0128955433566,0.2192213667622,-2.19307044856177));
#11092=CARTESIAN_POINT('Ctrl Pts',(97.0160336941558,0.276675806637948,-2.18732724918376));
#11093=CARTESIAN_POINT('Ctrl Pts',(97.019171844955,0.33383269456276,-2.17933192027265));
#11094=CARTESIAN_POINT('Ctrl Pts',(97.0223099957542,0.390505364565229,-2.16912921704673));
#11095=CARTESIAN_POINT('Ctrl Pts',(97.0263830606903,0.464061888708159,-2.15588693666489));
#11096=CARTESIAN_POINT('Ctrl Pts',(97.0304561256265,0.537085917159001,-2.13887335699214));
#11097=CARTESIAN_POINT('Ctrl Pts',(97.0345291905626,0.609161278881517,-2.11814506970402));
#11098=CARTESIAN_POINT('Ctrl Pts',(97.0385962713678,0.681130747767004,-2.09744723633379));
#11099=CARTESIAN_POINT('Ctrl Pts',(97.0426633521731,0.752153862088602,-2.07304566184749));
#11100=CARTESIAN_POINT('Ctrl Pts',(97.0467304329783,0.821823697525992,-2.04504811928343));
#11101=CARTESIAN_POINT('Ctrl Pts',(97.0507927553473,0.891412020084187,-2.01708333351133));
#11102=CARTESIAN_POINT('Ctrl Pts',(97.0548550777163,0.959649768653953,-1.98553111562693));
#11103=CARTESIAN_POINT('Ctrl Pts',(97.0589174000853,1.02614584808455,-1.95054881980914));
#11104=CARTESIAN_POINT('Ctrl Pts',(97.0629771442248,1.0925997245233,-1.91558872616564));
#11105=CARTESIAN_POINT('Ctrl Pts',(97.0670368883643,1.15731370385263,-1.87720309627234));
#11106=CARTESIAN_POINT('Ctrl Pts',(97.0710966325037,1.21991856752921,-1.8355965484271));
#11107=CARTESIAN_POINT('Ctrl Pts',(97.0751551119589,1.28250392865033,-1.79400296177942));
#11108=CARTESIAN_POINT('Ctrl Pts',(97.0792135914141,1.34298108122692,-1.74919071344024));
#11109=CARTESIAN_POINT('Ctrl Pts',(97.0832720708693,1.40100862152683,-1.70140848781458));
#11110=CARTESIAN_POINT('Ctrl Pts',(97.0873305975019,1.45903683636136,-1.65362570674981));
#11111=CARTESIAN_POINT('Ctrl Pts',(97.0913891241344,1.51461501493786,-1.60287318473939));
#11112=CARTESIAN_POINT('Ctrl Pts',(97.095447650767,1.56743503011681,-1.54943971369096));
#11113=CARTESIAN_POINT('Ctrl Pts',(97.0995103277522,1.62030906038859,-1.4959516002141));
#11114=CARTESIAN_POINT('Ctrl Pts',(97.1035730047375,1.67041895834268,-1.43977740318065));
#11115=CARTESIAN_POINT('Ctrl Pts',(97.1076356817227,1.71749421757976,-1.38124205430478));
#11116=CARTESIAN_POINT('Ctrl Pts',(97.1117004806999,1.76459406487082,-1.32267613161283));
#11117=CARTESIAN_POINT('Ctrl Pts',(97.1157652796771,1.80865583695665,-1.26174698841172));
#11118=CARTESIAN_POINT('Ctrl Pts',(97.1198300786543,1.84945162573308,-1.19880969468605));
#11119=CARTESIAN_POINT('Ctrl Pts',(97.1239021388965,1.89032029118394,-1.13575997120228));
#11120=CARTESIAN_POINT('Ctrl Pts',(97.1279741991386,1.92791108059944,-1.07069534584733));
#11121=CARTESIAN_POINT('Ctrl Pts',(97.1320462593808,1.96204164812848,-1.00399630029662));
#11122=CARTESIAN_POINT('Ctrl Pts',(97.1351844101783,1.98834451727579,-0.952594393021613));
#11123=CARTESIAN_POINT('Ctrl Pts',(97.1383225609758,2.01259326484021,-0.900222326425294));
#11124=CARTESIAN_POINT('Ctrl Pts',(97.1414607117732,2.03472436786831,-0.847061241471294));
#11125=CARTESIAN_POINT('Ctrl Pts',(97.145533776709,2.06344874268377,-0.778062469567536));
#11126=CARTESIAN_POINT('Ctrl Pts',(97.1496068416448,2.08871484518926,-0.707467889834191));
#11127=CARTESIAN_POINT('Ctrl Pts',(97.1536799065806,2.1103447503495,-0.635657954148531));
#11128=CARTESIAN_POINT('Ctrl Pts',(97.1577469873855,2.13194287693844,-0.563953521337008));
#11129=CARTESIAN_POINT('Ctrl Pts',(97.1618140681903,2.14991527623945,-0.491037731086796));
#11130=CARTESIAN_POINT('Ctrl Pts',(97.1658811489952,2.16413205091675,-0.417310994577013));
#11131=CARTESIAN_POINT('Ctrl Pts',(97.1699434713639,2.17833219213671,-0.343670517472408));
#11132=CARTESIAN_POINT('Ctrl Pts',(97.1740057937325,2.18878534873056,-0.269221445620318));
#11133=CARTESIAN_POINT('Ctrl Pts',(97.1780681161012,2.19541187259309,-0.194377749954301));
#11134=CARTESIAN_POINT('Ctrl Pts',(97.1821278602403,2.20203419080719,-0.119581555252327));
#11135=CARTESIAN_POINT('Ctrl Pts',(97.1861876043794,2.20483465367082,-0.0443917081330866));
#11136=CARTESIAN_POINT('Ctrl Pts',(97.1902473485185,2.20378519149202,0.0307705989617547));
#11137=CARTESIAN_POINT('Ctrl Pts',(97.1943058279734,2.20273605623982,0.105909491628809));
#11138=CARTESIAN_POINT('Ctrl Pts',(97.1983643074282,2.19783938380886,0.181020384202449));
#11139=CARTESIAN_POINT('Ctrl Pts',(97.2024227868831,2.18911921245078,0.255681586507276));
#11140=CARTESIAN_POINT('Ctrl Pts',(97.2064813135153,2.18039893972605,0.330343656702817));
#11141=CARTESIAN_POINT('Ctrl Pts',(97.2105398401475,2.16785513699549,0.404555552221366));
#11142=CARTESIAN_POINT('Ctrl Pts',(97.2145983667797,2.1515635825754,0.477901820602631));
#11143=CARTESIAN_POINT('Ctrl Pts',(97.2186610437646,2.13525536799677,0.551323094746271));
#11144=CARTESIAN_POINT('Ctrl Pts',(97.2227237207495,2.11519185211197,0.623876506897386));
#11145=CARTESIAN_POINT('Ctrl Pts',(97.2267863977345,2.09149957222474,0.695158643320879));
#11146=CARTESIAN_POINT('Ctrl Pts',(97.2308511967113,2.06779491753456,0.766478011382557));
#11147=CARTESIAN_POINT('Ctrl Pts',(97.2349159956882,2.04045789817965,0.836524336214279));
#11148=CARTESIAN_POINT('Ctrl Pts',(97.238980794665,2.0096634631363,0.904913678167703));
#11149=CARTESIAN_POINT('Ctrl Pts',(97.2430528549069,1.97881401761057,0.973425189295053));
#11150=CARTESIAN_POINT('Ctrl Pts',(97.2471249151487,1.94449503820559,1.040273379795));
#11151=CARTESIAN_POINT('Ctrl Pts',(97.2511969753905,1.90692751884061,1.1050988362533));
#11152=CARTESIAN_POINT('Ctrl Pts',(97.2543351261912,1.87797594789814,1.15505685406376));
#11153=CARTESIAN_POINT('Ctrl Pts',(97.2574732769918,1.84709599841897,1.2038140468137));
#11154=CARTESIAN_POINT('Ctrl Pts',(97.2606114277925,1.81440550029416,1.25121887793555));
#11155=CARTESIAN_POINT('Ctrl Pts',(97.2646637681727,1.77219177825978,1.31243343503482));
#11156=CARTESIAN_POINT('Ctrl Pts',(97.2687161085529,1.72679109134377,1.37163325595954));
#11157=CARTESIAN_POINT('Ctrl Pts',(97.2727684489331,1.67842324522032,1.42846470376558));
#11158=CARTESIAN_POINT('Ctrl Pts',(97.2768148242482,1.63012659680576,1.48521249539917));
#11159=CARTESIAN_POINT('Ctrl Pts',(97.2808611995633,1.5788717685914,1.53959846900412));
#11160=CARTESIAN_POINT('Ctrl Pts',(97.2849075748784,1.52492150538961,1.59129833859032));
#11161=CARTESIAN_POINT('Ctrl Pts',(97.2889492578127,1.47103380563322,1.642938254401));
#11162=CARTESIAN_POINT('Ctrl Pts',(97.292990940747,1.41445722629823,1.69189792081092));
#11163=CARTESIAN_POINT('Ctrl Pts',(97.2970326236813,1.35549325620361,1.73788780776739));
#11164=CARTESIAN_POINT('Ctrl Pts',(97.3010718017673,1.29656582925137,1.78384919231833));
#11165=CARTESIAN_POINT('Ctrl Pts',(97.3051109798534,1.23525432669,1.82684415250284));
#11166=CARTESIAN_POINT('Ctrl Pts',(97.3091501579395,1.17189432754206,1.86662253417094));
#11167=CARTESIAN_POINT('Ctrl Pts',(97.3131881726005,1.1085525782978,1.90638945826891));
#11168=CARTESIAN_POINT('Ctrl Pts',(97.3172261872615,1.04316391258803,1.94294138651562));
#11169=CARTESIAN_POINT('Ctrl Pts',(97.3212642019225,0.976092579314091,1.9760716780036));
#11170=CARTESIAN_POINT('Ctrl Pts',(97.3253023929626,0.909018316386416,2.00920341661179));
#11171=CARTESIAN_POINT('Ctrl Pts',(97.3293405840028,0.840261674001143,2.03891301004312));
#11172=CARTESIAN_POINT('Ctrl Pts',(97.3333787750429,0.770209643490197,2.06504070300677));
#11173=CARTESIAN_POINT('Ctrl Pts',(97.3374210894093,0.700086084075982,2.09119507450078));
#11174=CARTESIAN_POINT('Ctrl Pts',(97.3414634037757,0.628664949918502,2.11376007679749));
#11175=CARTESIAN_POINT('Ctrl Pts',(97.3455057181421,0.556350434859627,2.13262518826715));
#11176=CARTESIAN_POINT('Ctrl Pts',(97.3495503257518,0.48399489509044,2.15150100209349));
#11177=CARTESIAN_POINT('Ctrl Pts',(97.3535949333615,0.41074543875725,2.16667265050363));
#11178=CARTESIAN_POINT('Ctrl Pts',(97.3576395409712,0.337015916512282,2.17808086902608));
#11179=CARTESIAN_POINT('Ctrl Pts',(97.3616909554316,0.263162311562423,2.18950828694883));
#11180=CARTESIAN_POINT('Ctrl Pts',(97.365742369892,0.188827508213047,2.1971595846685));
#11181=CARTESIAN_POINT('Ctrl Pts',(97.3697937843524,0.114429203377559,2.20102747766001));
#11182=CARTESIAN_POINT('Ctrl Pts',(97.3718786584933,0.0761435371257581,
2.20301791091649));
#11183=CARTESIAN_POINT('Ctrl Pts',(97.3739635326342,0.0378410376971126,
2.20400728289753));
#11184=CARTESIAN_POINT('Ctrl Pts',(97.3760484067751,-0.000421831323937878,
2.20399995963211));
#11185=CARTESIAN_POINT('',(98.1260484067631,0.00200370534590846,2.2039990891933));
#11186=CARTESIAN_POINT('Ctrl Pts',(97.3760484068025,-0.00042183182640112,
2.20399995963201));
#11187=CARTESIAN_POINT('Ctrl Pts',(97.3772863191389,-0.023140746438742,
2.20399561137365));
#11188=CARTESIAN_POINT('Ctrl Pts',(97.3785242314752,-0.0458559000617912,
2.20363999219748));
#11189=CARTESIAN_POINT('Ctrl Pts',(97.3797621438116,-0.0685600735653428,
2.20293338898677));
#11190=CARTESIAN_POINT('Ctrl Pts',(97.3838352087488,-0.143262918273813,
2.20060847414624));
#11191=CARTESIAN_POINT('Ctrl Pts',(97.387908273686,-0.217991429363417,2.19447493865576));
#11192=CARTESIAN_POINT('Ctrl Pts',(97.3919813386232,-0.292325635221059,
2.18452780320888));
#11193=CARTESIAN_POINT('Ctrl Pts',(97.3960484194294,-0.36655062955683,2.17459528205414));
#11194=CARTESIAN_POINT('Ctrl Pts',(97.4001155002357,-0.440381999516932,
2.16086034783918));
#11195=CARTESIAN_POINT('Ctrl Pts',(97.4041825810419,-0.513401423440742,
2.14337000501757));
#11196=CARTESIAN_POINT('Ctrl Pts',(97.408244903412,-0.586335415506716,2.12590012568912));
#11197=CARTESIAN_POINT('Ctrl Pts',(97.4123072257821,-0.658458886911531,
2.10468367785998));
#11198=CARTESIAN_POINT('Ctrl Pts',(97.4163695481522,-0.729361911800216,
2.07981903097725));
#11199=CARTESIAN_POINT('Ctrl Pts',(97.4204292922927,-0.800219936745927,
2.05497016491196));
#11200=CARTESIAN_POINT('Ctrl Pts',(97.4244890364332,-0.869858602827608,
2.02647785205489));
#11201=CARTESIAN_POINT('Ctrl Pts',(97.4285487805737,-0.93788270160062,1.99449042064341));
#11202=CARTESIAN_POINT('Ctrl Pts',(97.4326072600299,-1.00588560962769,1.96251295389952));
#11203=CARTESIAN_POINT('Ctrl Pts',(97.4366657394862,-1.07227451717383,1.9270427333978));
#11204=CARTESIAN_POINT('Ctrl Pts',(97.4407242189425,-1.13667527580074,1.88827575247455));
#11205=CARTESIAN_POINT('Ctrl Pts',(97.444782745576,-1.20107678304696,1.84950832090892));
#11206=CARTESIAN_POINT('Ctrl Pts',(97.4488412722096,-1.26348968734669,1.80744430060874));
#11207=CARTESIAN_POINT('Ctrl Pts',(97.4528997988432,-1.32356688299169,1.76232423414298));
#11208=CARTESIAN_POINT('Ctrl Pts',(97.4569624758295,-1.38370551510689,1.71715802674823));
#11209=CARTESIAN_POINT('Ctrl Pts',(97.4610251528158,-1.44150328613208,1.66892981972681));
#11210=CARTESIAN_POINT('Ctrl Pts',(97.4650878298021,-1.49664501156592,1.61792141631009));
#11211=CARTESIAN_POINT('Ctrl Pts',(97.4691526287803,-1.55181553827964,1.5668863705043));
#11212=CARTESIAN_POINT('Ctrl Pts',(97.4732174277585,-1.6043269229983,1.51306857857434));
#11213=CARTESIAN_POINT('Ctrl Pts',(97.4772822267367,-1.65390170539555,1.45678589672254));
#11214=CARTESIAN_POINT('Ctrl Pts',(97.4813542869799,-1.70356504706262,1.40040267276108));
#11215=CARTESIAN_POINT('Ctrl Pts',(97.485426347223,-1.7502810108955,1.34154613831157));
#11216=CARTESIAN_POINT('Ctrl Pts',(97.4894984074662,-1.79381348507808,1.28056596110939));
#11217=CARTESIAN_POINT('Ctrl Pts',(97.4926365582544,-1.82736197405157,1.23357132455627));
#11218=CARTESIAN_POINT('Ctrl Pts',(97.4957747090425,-1.85902060639208,1.18531610622014));
#11219=CARTESIAN_POINT('Ctrl Pts',(97.4989128598307,-1.88870001086929,1.13597018840388));
#11220=CARTESIAN_POINT('Ctrl Pts',(97.5029859247648,-1.9272214681866,1.07192319351211));
#11221=CARTESIAN_POINT('Ctrl Pts',(97.5070589896989,-1.96255570848192,1.00579103732401));
#11222=CARTESIAN_POINT('Ctrl Pts',(97.5111320546331,-1.99447099743568,0.937924005657145));
#11223=CARTESIAN_POINT('Ctrl Pts',(97.5151991354363,-2.02633939657287,0.870156683965339));
#11224=CARTESIAN_POINT('Ctrl Pts',(97.5192662162395,-2.05479861579184,0.800659975828997));
#11225=CARTESIAN_POINT('Ctrl Pts',(97.5233332970427,-2.07966150680036,0.729810946158569));
#11226=CARTESIAN_POINT('Ctrl Pts',(97.5273956194097,-2.10449530852207,0.659044809010307));
#11227=CARTESIAN_POINT('Ctrl Pts',(97.5314579417767,-2.12574098438867,0.586929942059288));
#11228=CARTESIAN_POINT('Ctrl Pts',(97.5355202641437,-2.14325910710736,0.513864184197897));
#11229=CARTESIAN_POINT('Ctrl Pts',(97.5395800082812,-2.16076611161887,0.440844798898597));
#11230=CARTESIAN_POINT('Ctrl Pts',(97.5436397524187,-2.17455014654319,0.366876183396631));
#11231=CARTESIAN_POINT('Ctrl Pts',(97.5476994965561,-2.18452174885648,0.292370875384411));
#11232=CARTESIAN_POINT('Ctrl Pts',(97.5517579760094,-2.19449024483403,0.217888777132598));
#11233=CARTESIAN_POINT('Ctrl Pts',(97.5558164554626,-2.20064860291723,0.142870791250414));
#11234=CARTESIAN_POINT('Ctrl Pts',(97.5598749349159,-2.20295883306561,0.0677375805460152));
#11235=CARTESIAN_POINT('Ctrl Pts',(97.5639334615465,-2.205269090069,-0.00739650353620468));
#11236=CARTESIAN_POINT('Ctrl Pts',(97.567991988177,-2.20373111743813,-0.0826453378098284));
#11237=CARTESIAN_POINT('Ctrl Pts',(97.5720505148076,-2.19835902081088,-0.157586851035928));
#11238=CARTESIAN_POINT('Ctrl Pts',(97.576113191791,-2.19298143054075,-0.232605001362973));
#11239=CARTESIAN_POINT('Ctrl Pts',(97.5801758687743,-2.18376192072935,-0.307314725757909));
#11240=CARTESIAN_POINT('Ctrl Pts',(97.5842385457576,-2.17076657192755,-0.381298426697426));
#11241=CARTESIAN_POINT('Ctrl Pts',(97.5883033447329,-2.15776443547665,-0.455320770339663));
#11242=CARTESIAN_POINT('Ctrl Pts',(97.5923681437082,-2.14098263930786,-0.52861586951254));
#11243=CARTESIAN_POINT('Ctrl Pts',(97.5964329426835,-2.12053800601775,-0.600778299403589));
#11244=CARTESIAN_POINT('Ctrl Pts',(97.6005050029238,-2.10005685089683,-0.67306963862836));
#11245=CARTESIAN_POINT('Ctrl Pts',(97.6045770631641,-2.0758999428233,-0.744223814250836));
#11246=CARTESIAN_POINT('Ctrl Pts',(97.6086491234044,-2.0482332452747,-0.813852918500303));
#11247=CARTESIAN_POINT('Ctrl Pts',(97.6117872742196,-2.02691178529126,-0.867512888481555));
#11248=CARTESIAN_POINT('Ctrl Pts',(97.6149254250347,-2.003506850464,-0.920267453980305));
#11249=CARTESIAN_POINT('Ctrl Pts',(97.6180635758498,-1.97811280272008,-0.971949453271568));
#11250=CARTESIAN_POINT('Ctrl Pts',(97.6221366407851,-1.94515339078515,-1.03902849169189));
#11251=CARTESIAN_POINT('Ctrl Pts',(97.6262097057203,-1.90871451324376,-1.10455847585856));
#11252=CARTESIAN_POINT('Ctrl Pts',(97.6302827706556,-1.86896502488545,-1.16815484237105));
#11253=CARTESIAN_POINT('Ctrl Pts',(97.6343498514599,-1.82927393631882,-1.23165777335243));
#11254=CARTESIAN_POINT('Ctrl Pts',(97.6384169322642,-1.78628214479456,-1.29323232543297));
#11255=CARTESIAN_POINT('Ctrl Pts',(97.6424840130685,-1.7402051703996,-1.35251690004764));
#11256=CARTESIAN_POINT('Ctrl Pts',(97.6465463354365,-1.69418210551725,-1.41173211241437));
#11257=CARTESIAN_POINT('Ctrl Pts',(97.6506086578046,-1.64508132079815,-1.46866229527368));
#11258=CARTESIAN_POINT('Ctrl Pts',(97.6546709801727,-1.59316165295788,-1.52297470351432));
#11259=CARTESIAN_POINT('Ctrl Pts',(97.6587307243112,-1.54127493691497,-1.57725264135973));
#11260=CARTESIAN_POINT('Ctrl Pts',(97.6627904684497,-1.48657321703343,-1.62891575723723));
#11261=CARTESIAN_POINT('Ctrl Pts',(97.6668502125881,-1.42935475595175,-1.67766533660266));
#11262=CARTESIAN_POINT('Ctrl Pts',(97.6709086920424,-1.37215411946322,-1.72639972958589));
#11263=CARTESIAN_POINT('Ctrl Pts',(97.6749671714966,-1.31243866159608,-1.77222207865274));
#11264=CARTESIAN_POINT('Ctrl Pts',(97.6790256509508,-1.25054136322061,-1.81487252964894));
#11265=CARTESIAN_POINT('Ctrl Pts',(97.6830841775824,-1.1886433453272,-1.85752347643034));
#11266=CARTESIAN_POINT('Ctrl Pts',(97.6871427042139,-1.12456383074711,-1.89700218249863));
#11267=CARTESIAN_POINT('Ctrl Pts',(97.6912012308455,-1.05866521063653,-1.93309181669881));
#11268=CARTESIAN_POINT('Ctrl Pts',(97.6952639078297,-0.99269920091883,-1.969218357078));
#11269=CARTESIAN_POINT('Ctrl Pts',(97.6993265848139,-0.924910790533539,
-2.00194867482967));
#11270=CARTESIAN_POINT('Ctrl Pts',(97.7033892617981,-0.855686771579625,
-2.03111204736313));
#11271=CARTESIAN_POINT('Ctrl Pts',(97.7074540607743,-0.786426595970732,
-2.06029065232623));
#11272=CARTESIAN_POINT('Ctrl Pts',(97.7115188597505,-0.715729767899791,
-2.08589843920142));
#11273=CARTESIAN_POINT('Ctrl Pts',(97.7155836587266,-0.644000341454866,
-2.10781392921814));
#11274=CARTESIAN_POINT('Ctrl Pts',(97.7196557189678,-0.572142779184829,
-2.12976856857057));
#11275=CARTESIAN_POINT('Ctrl Pts',(97.7237277792089,-0.499249397928626,
-2.14801762026816));
#11276=CARTESIAN_POINT('Ctrl Pts',(97.72779983945,-0.425736154340295,-2.16249039925904));
#11277=CARTESIAN_POINT('Ctrl Pts',(97.7309379902564,-0.369082855768432,
-2.17364390887598));
#11278=CARTESIAN_POINT('Ctrl Pts',(97.7340761410627,-0.312061674981444,
-2.18255570322988));
#11279=CARTESIAN_POINT('Ctrl Pts',(97.737214291869,-0.254864237668701,-2.18921452131982));
#11280=CARTESIAN_POINT('Ctrl Pts',(97.741287356814,-0.180626608172958,-2.19785712653895));
#11281=CARTESIAN_POINT('Ctrl Pts',(97.745360421759,-0.105805703914654,-2.20273595165285));
#11282=CARTESIAN_POINT('Ctrl Pts',(97.749433486704,-0.0308162371980697,
-2.20378455379036));
#11283=CARTESIAN_POINT('Ctrl Pts',(97.7535005675181,0.0440630552907173,
-2.20483161532574));
#11284=CARTESIAN_POINT('Ctrl Pts',(97.7575676483323,0.11910994509809,-2.20205961984711));
#11285=CARTESIAN_POINT('Ctrl Pts',(97.7616347291464,0.193903737515108,-2.19545378921481));
#11286=CARTESIAN_POINT('Ctrl Pts',(97.7656970515243,0.26861002208437,-2.1888556873258));
#11287=CARTESIAN_POINT('Ctrl Pts',(97.7697593739022,0.343063324368703,-2.17843270382538));
#11288=CARTESIAN_POINT('Ctrl Pts',(97.7738216962801,0.416843730981485,-2.16422210134298));
#11289=CARTESIAN_POINT('Ctrl Pts',(97.7778814404284,0.490577311466708,-2.15002051788766));
#11290=CARTESIAN_POINT('Ctrl Pts',(97.7819411845768,0.563638376091331,-2.13203617577166));
#11291=CARTESIAN_POINT('Ctrl Pts',(97.7860009287251,0.635614252189,-2.11035791334414));
#11292=CARTESIAN_POINT('Ctrl Pts',(97.7900594081892,0.707567706489905,-2.08868640409033));
#11293=CARTESIAN_POINT('Ctrl Pts',(97.7941178876532,0.778436186583184,-2.06332339684287));
#11294=CARTESIAN_POINT('Ctrl Pts',(97.7981763671173,0.847820870684519,-2.03440796578065));
#11295=CARTESIAN_POINT('Ctrl Pts',(97.8022348937587,0.917206361339779,-2.00549219859447));
#11296=CARTESIAN_POINT('Ctrl Pts',(97.8062934204001,0.985107581724493,-1.97302411092295));
#11297=CARTESIAN_POINT('Ctrl Pts',(97.8103519470415,1.05114593553944,-1.93719080686414));
#11298=CARTESIAN_POINT('Ctrl Pts',(97.8144146240354,1.11725182185513,-1.90132085875693));
#11299=CARTESIAN_POINT('Ctrl Pts',(97.8184773010294,1.1814906168022,-1.86207905029068));
#11300=CARTESIAN_POINT('Ctrl Pts',(97.8225399780234,1.24350925713102,-1.8196979769812));
#11301=CARTESIAN_POINT('Ctrl Pts',(97.8266047770093,1.30556029064606,-1.77729476745601));
#11302=CARTESIAN_POINT('Ctrl Pts',(97.8306695759951,1.36538848002121,-1.73174931730094));
#11303=CARTESIAN_POINT('Ctrl Pts',(97.834734374981,1.42267279825242,-1.68333541194636));
#11304=CARTESIAN_POINT('Ctrl Pts',(97.8388064352317,1.48005944789153,-1.63483502108843));
#11305=CARTESIAN_POINT('Ctrl Pts',(97.8428784954824,1.53489280054329,-1.58345626689899));
#11306=CARTESIAN_POINT('Ctrl Pts',(97.8469505557331,1.58688807197544,-1.52951045992569));
#11307=CARTESIAN_POINT('Ctrl Pts',(97.8500887064514,1.6269584511819,-1.48793689212848));
#11308=CARTESIAN_POINT('Ctrl Pts',(97.8532268571698,1.66534400792165,-1.44483951419821));
#11309=CARTESIAN_POINT('Ctrl Pts',(97.8563650078881,1.70193145066577,-1.4003732849618));
#11310=CARTESIAN_POINT('Ctrl Pts',(97.8604380728076,1.74941898167051,-1.34265972858413));
#11311=CARTESIAN_POINT('Ctrl Pts',(97.8645111377271,1.7940591075753,-1.28241663984275));
#11312=CARTESIAN_POINT('Ctrl Pts',(97.8685842026466,1.83557128389276,-1.21995658191113));
#11313=CARTESIAN_POINT('Ctrl Pts',(97.8726512834352,1.87702247068463,-1.15758829005009));
#11314=CARTESIAN_POINT('Ctrl Pts',(97.8767183642239,1.91535456988331,-1.09300989014078));
#11315=CARTESIAN_POINT('Ctrl Pts',(97.8807854450125,1.95032721951919,-1.02656696654556));
#11316=CARTESIAN_POINT('Ctrl Pts',(97.884847767365,1.98525895157162,-0.960201780379423));
#11317=CARTESIAN_POINT('Ctrl Pts',(97.8889100897175,2.01683882182788,-0.891976824994816));
#11318=CARTESIAN_POINT('Ctrl Pts',(97.8929724120701,2.04487063161971,-0.822265224814485));
#11319=CARTESIAN_POINT('Ctrl Pts',(97.8970321561931,2.07288465049487,-0.752597868415728));
#11320=CARTESIAN_POINT('Ctrl Pts',(97.9010919003162,2.09735489976669,-0.681446181414142));
#11321=CARTESIAN_POINT('Ctrl Pts',(97.9051516444392,2.11813245303143,-0.609205147232894));
#11322=CARTESIAN_POINT('Ctrl Pts',(97.9092101238781,2.13890353371035,-0.536986617448005));
#11323=CARTESIAN_POINT('Ctrl Pts',(97.9132686033171,2.15598407044871,-0.463679872810791));
#11324=CARTESIAN_POINT('Ctrl Pts',(97.9173270827559,2.16927486445895,-0.389695473962193));
#11325=CARTESIAN_POINT('Ctrl Pts',(97.9213856093723,2.18256581296693,-0.315710215087998));
#11326=CARTESIAN_POINT('Ctrl Pts',(97.9254441359887,2.1920668486204,-0.241047756616787));
#11327=CARTESIAN_POINT('Ctrl Pts',(97.929502662605,2.1977301000837,-0.166127683382604));
#11328=CARTESIAN_POINT('Ctrl Pts',(97.9335653395744,2.20339914293265,-0.0911309949673516));
#11329=CARTESIAN_POINT('Ctrl Pts',(97.9376280165438,2.20522252828817,-0.0158766428677534));
#11330=CARTESIAN_POINT('Ctrl Pts',(97.9416906935132,2.20320445441821,0.0592126002784699));
#11331=CARTESIAN_POINT('Ctrl Pts',(97.9457554924746,2.20118532648051,0.134341063569739));
#11332=CARTESIAN_POINT('Ctrl Pts',(97.9498202914361,2.19532078094752,0.209303769722548));
#11333=CARTESIAN_POINT('Ctrl Pts',(97.9538850903976,2.18566699386736,0.283682554836975));
#11334=CARTESIAN_POINT('Ctrl Pts',(97.9579571506244,2.17599596147924,0.358194208539071));
#11335=CARTESIAN_POINT('Ctrl Pts',(97.9620292108512,2.16252225269991,0.432119387265153));
#11336=CARTESIAN_POINT('Ctrl Pts',(97.9661012710781,2.14535322029897,0.505050057076367));
#11337=CARTESIAN_POINT('Ctrl Pts',(97.9692394220212,2.13212183072731,0.561254395297625));
#11338=CARTESIAN_POINT('Ctrl Pts',(97.9723775729642,2.11669681584981,0.616868281523678));
#11339=CARTESIAN_POINT('Ctrl Pts',(97.9755157239073,2.09914703400378,0.671712534967985));
#11340=CARTESIAN_POINT('Ctrl Pts',(97.9795887888431,2.07636884316304,0.742895919606782));
#11341=CARTESIAN_POINT('Ctrl Pts',(97.9836618537789,2.04992181246092,0.813056629302231));
#11342=CARTESIAN_POINT('Ctrl Pts',(97.9877349187148,2.01991664467316,0.881789514891353));
#11343=CARTESIAN_POINT('Ctrl Pts',(97.9918019995195,1.98995556036083,0.950421418393163));
#11344=CARTESIAN_POINT('Ctrl Pts',(97.9958690803242,1.95644690732366,1.01762922873601));
#11345=CARTESIAN_POINT('Ctrl Pts',(97.9999361611289,1.9195509141684,1.0830236783724));
#11346=CARTESIAN_POINT('Ctrl Pts',(98.0039984834971,1.88269808888879,1.14834161727606));
#11347=CARTESIAN_POINT('Ctrl Pts',(98.0080608058654,1.8424660308018,1.21184999687947));
#11348=CARTESIAN_POINT('Ctrl Pts',(98.0121231282336,1.79906204435868,1.27318174686412));
#11349=CARTESIAN_POINT('Ctrl Pts',(98.0161828723722,1.75568560507644,1.33447457149368));
#11350=CARTESIAN_POINT('Ctrl Pts',(98.0202426165107,1.7091415073808,1.39359311907142));
#11351=CARTESIAN_POINT('Ctrl Pts',(98.0243023606492,1.65968104116966,1.45019820768818));
#11352=CARTESIAN_POINT('Ctrl Pts',(98.0283608401034,1.61023598279663,1.50678566278652));
#11353=CARTESIAN_POINT('Ctrl Pts',(98.0324193195575,1.55787667365686,1.56086085420544));
#11354=CARTESIAN_POINT('Ctrl Pts',(98.0364777990116,1.50289443965292,1.61211795575272));
#11355=CARTESIAN_POINT('Ctrl Pts',(98.0405363256429,1.44791156651626,1.66337565313048));
#11356=CARTESIAN_POINT('Ctrl Pts',(98.0445948522743,1.39030605843857,1.71181487132733));
#11357=CARTESIAN_POINT('Ctrl Pts',(98.0486533789056,1.33040463637171,1.75716803508392));
#11358=CARTESIAN_POINT('Ctrl Pts',(98.0527160558894,1.27044195758822,1.80256757813844));
#11359=CARTESIAN_POINT('Ctrl Pts',(98.0567787328732,1.20817905778068,1.8448744757943));
#11360=CARTESIAN_POINT('Ctrl Pts',(98.060841409857,1.14397354961176,1.88386318977485));
#11361=CARTESIAN_POINT('Ctrl Pts',(98.0649062088326,1.07973450602679,1.92287226809457));
#11362=CARTESIAN_POINT('Ctrl Pts',(98.0689710078082,1.01355125415047,1.95855948455254));
#11363=CARTESIAN_POINT('Ctrl Pts',(98.0730358067838,0.945805695656618,1.99074548500392));
#11364=CARTESIAN_POINT('Ctrl Pts',(98.0771078670242,0.877939118032233,2.02298898179715));
#11365=CARTESIAN_POINT('Ctrl Pts',(98.0811799272646,0.808505101086245,2.05171858690034));
#11366=CARTESIAN_POINT('Ctrl Pts',(98.085251987505,0.737904760917371,2.07680344852744));
#11367=CARTESIAN_POINT('Ctrl Pts',(98.0883901383121,0.683496303919378,2.09613520545488));
#11368=CARTESIAN_POINT('Ctrl Pts',(98.0915282891192,0.628395567240788,2.11330331419059));
#11369=CARTESIAN_POINT('Ctrl Pts',(98.0946664399263,0.572790460130373,2.1282685659436));
#11370=CARTESIAN_POINT('Ctrl Pts',(98.0998967677324,0.480113926796354,2.15321101682651));
#11371=CARTESIAN_POINT('Ctrl Pts',(98.1051270955386,0.385747273566499,2.17211193581593));
#11372=CARTESIAN_POINT('Ctrl Pts',(98.1103574233447,0.290381856862663,2.18478703245991));
#11373=CARTESIAN_POINT('Ctrl Pts',(98.1155877511508,0.195016440158827,2.19746212910389));
#11374=CARTESIAN_POINT('Ctrl Pts',(98.120818078957,0.0986519424616607,2.20391122409829));
#11375=CARTESIAN_POINT('Ctrl Pts',(98.1260484067631,0.00200370534589378,
2.2039990891933));
#11376=CARTESIAN_POINT('',(98.8760484068365,-0.000689329991712772,2.20399989220149));
#11377=CARTESIAN_POINT('Ctrl Pts',(98.1260484068025,0.00200370461793977,
2.20399908919396));
#11378=CARTESIAN_POINT('Ctrl Pts',(98.1300685156377,-0.0722815880720076,
2.20406662360663));
#11379=CARTESIAN_POINT('Ctrl Pts',(98.1340886244729,-0.146655895447738,
2.20037424384966));
#11380=CARTESIAN_POINT('Ctrl Pts',(98.1381087333081,-0.220704688647699,
2.1929216676409));
#11381=CARTESIAN_POINT('Ctrl Pts',(98.1421265750994,-0.294711723807198,
2.1854732941337));
#11382=CARTESIAN_POINT('Ctrl Pts',(98.1461444168907,-0.36839312409481,2.17426897856647));
#11383=CARTESIAN_POINT('Ctrl Pts',(98.1501622586819,-0.441337082029862,
2.15936045625212));
#11384=CARTESIAN_POINT('Ctrl Pts',(98.1541791980949,-0.514264657277744,
2.14445528228442));
#11385=CARTESIAN_POINT('Ctrl Pts',(98.1581961375079,-0.58645464080003,2.12584765095944));
#11386=CARTESIAN_POINT('Ctrl Pts',(98.1622130769208,-0.657504793743489,
2.103640522096));
#11387=CARTESIAN_POINT('Ctrl Pts',(98.1662304772368,-0.728563098969988,
2.0814308451902));
#11388=CARTESIAN_POINT('Ctrl Pts',(98.1702478775528,-0.798480849007217,
2.05562099963288));
#11389=CARTESIAN_POINT('Ctrl Pts',(98.1742652778687,-0.866872050191152,
2.02636345421975));
#11390=CARTESIAN_POINT('Ctrl Pts',(98.1782870082842,-0.935336965888348,
1.99707437396467));
#11391=CARTESIAN_POINT('Ctrl Pts',(98.1823087386997,-1.00227160142837,1.9643303742205));
#11392=CARTESIAN_POINT('Ctrl Pts',(98.1863304691151,-1.06731191668464,1.92833121441908));
#11393=CARTESIAN_POINT('Ctrl Pts',(98.1903547887712,-1.13239410571263,1.89230887790651));
#11394=CARTESIAN_POINT('Ctrl Pts',(98.1943791084272,-1.19557913579793,1.85302747234195));
#11395=CARTESIAN_POINT('Ctrl Pts',(98.1984034280833,-1.25653177887033,1.8107302086973));
#11396=CARTESIAN_POINT('Ctrl Pts',(98.20243433856,-1.31758424700099,1.76836367280136));
#11397=CARTESIAN_POINT('Ctrl Pts',(98.2064652490368,-1.3763966527891,1.72297172740696));
#11398=CARTESIAN_POINT('Ctrl Pts',(98.2104961595136,-1.4326674162586,1.6748373277399));
#11399=CARTESIAN_POINT('Ctrl Pts',(98.2116031583243,-1.44812091456723,1.66161829856775));
#11400=CARTESIAN_POINT('Ctrl Pts',(98.2127101571349,-1.46338294330759,1.64819263968996));
#11401=CARTESIAN_POINT('Ctrl Pts',(98.2138171559455,-1.47844777324369,1.6345666648353));
#11402=CARTESIAN_POINT('Ctrl Pts',(98.2178902207403,-1.53387694612193,1.58443158073162));
#11403=CARTESIAN_POINT('Ctrl Pts',(98.221963285535,-1.5868599519597,1.53137716195861));
#11404=CARTESIAN_POINT('Ctrl Pts',(98.2260363503298,-1.63707348818888,1.47567150621982));
#11405=CARTESIAN_POINT('Ctrl Pts',(98.2301034309937,-1.68721325088763,1.42004769301192));
#11406=CARTESIAN_POINT('Ctrl Pts',(98.2341705116576,-1.73459130536596,1.36178072807496));
#11407=CARTESIAN_POINT('Ctrl Pts',(98.2382375923216,-1.77891926122074,1.30117726004487));
#11408=CARTESIAN_POINT('Ctrl Pts',(98.2422999145501,-1.82319535390158,1.24064469734175));
#11409=CARTESIAN_POINT('Ctrl Pts',(98.2463622367787,-1.86442815744766,1.17778144618194));
#11410=CARTESIAN_POINT('Ctrl Pts',(98.2504245590073,-1.90236893434033,1.11292786722987));
#11411=CARTESIAN_POINT('Ctrl Pts',(98.2544843030069,-1.94028563140743,1.0481154488179));
#11412=CARTESIAN_POINT('Ctrl Pts',(98.2585440470065,-1.97491420741665,0.981315620368102));
#11413=CARTESIAN_POINT('Ctrl Pts',(98.2626037910061,-2.00604948532256,0.912897290190472));
#11414=CARTESIAN_POINT('Ctrl Pts',(98.2666622703222,-2.03717506402784,0.844500273556684));
#11415=CARTESIAN_POINT('Ctrl Pts',(98.2707207496383,-2.06480930761938,0.774486190542105));
#11416=CARTESIAN_POINT('Ctrl Pts',(98.2747792289545,-2.08879394854574,0.70324664273547));
#11417=CARTESIAN_POINT('Ctrl Pts',(98.2788377554489,-2.11277886828451,0.632006266795926));
#11418=CARTESIAN_POINT('Ctrl Pts',(98.2828962819433,-2.13311395047349,0.559540850854564));
#11419=CARTESIAN_POINT('Ctrl Pts',(98.2869548084377,-2.14969037951925,0.486258441780054));
#11420=CARTESIAN_POINT('Ctrl Pts',(98.2910174852873,-2.16628376005417,0.412901092200628));
#11421=CARTESIAN_POINT('Ctrl Pts',(98.2950801621368,-2.17911070622868,0.338725547815187));
#11422=CARTESIAN_POINT('Ctrl Pts',(98.2991428389864,-2.18811344346597,0.26415063604598));
#11423=CARTESIAN_POINT('Ctrl Pts',(98.3032076378291,-2.19712088295916,0.189536772754672));
#11424=CARTESIAN_POINT('Ctrl Pts',(98.3072724366717,-2.20230010289387,0.114523603452549));
#11425=CARTESIAN_POINT('Ctrl Pts',(98.3113372355144,-2.20364542091123,0.0395330102187932));
#11426=CARTESIAN_POINT('Ctrl Pts',(98.3154092956254,-2.20499314217548,-0.0355915445818049));
#11427=CARTESIAN_POINT('Ctrl Pts',(98.3194813557364,-2.20249329748571,-0.110692964854589));
#11428=CARTESIAN_POINT('Ctrl Pts',(98.3235534158474,-2.19619231302927,-0.185351892871758));
#11429=CARTESIAN_POINT('Ctrl Pts',(98.3266915678865,-2.19133643009012,-0.242888142535564));
#11430=CARTESIAN_POINT('Ctrl Pts',(98.3298297199256,-2.18422409221878,-0.300161630191771));
#11431=CARTESIAN_POINT('Ctrl Pts',(98.3329678719647,-2.17489716874867,-0.35698502121098));
#11432=CARTESIAN_POINT('Ctrl Pts',(98.3370409369447,-2.16279158403393,-0.430737140649556));
#11433=CARTESIAN_POINT('Ctrl Pts',(98.3411140019247,-2.14690693162874,-0.504015026224418));
#11434=CARTESIAN_POINT('Ctrl Pts',(98.3451870669046,-2.12729337414513,-0.576401683132722));
#11435=CARTESIAN_POINT('Ctrl Pts',(98.3492541477523,-2.10770863282881,-0.648681989828063));
#11436=CARTESIAN_POINT('Ctrl Pts',(98.3533212286001,-2.08440598731108,-0.720073210512294));
#11437=CARTESIAN_POINT('Ctrl Pts',(98.3573883094478,-2.05748691816683,-0.790166806169656));
#11438=CARTESIAN_POINT('Ctrl Pts',(98.3614506318572,-2.03059934402735,-0.860178393117225));
#11439=CARTESIAN_POINT('Ctrl Pts',(98.3655129542665,-2.00010392295595,-0.928894927886572));
#11440=CARTESIAN_POINT('Ctrl Pts',(98.3695752766759,-1.96615195503874,-0.995922933613512));
#11441=CARTESIAN_POINT('Ctrl Pts',(98.3736350208544,-1.93222153538971,-1.06290839872994));
#11442=CARTESIAN_POINT('Ctrl Pts',(98.3776947650329,-1.89483913738575,-1.12820703653688));
#11443=CARTESIAN_POINT('Ctrl Pts',(98.3817545092114,-1.85420365720231,-1.19144651479518));
#11444=CARTESIAN_POINT('Ctrl Pts',(98.3858129887042,-1.81358083572474,-1.25466629278289));
#11445=CARTESIAN_POINT('Ctrl Pts',(98.3898714681971,-1.76970720206007,-1.3158277834051));
#11446=CARTESIAN_POINT('Ctrl Pts',(98.39392994769,-1.72282614248017,-1.37458578589584));
#11447=CARTESIAN_POINT('Ctrl Pts',(98.3979884743588,-1.67594453795309,-1.4333444713918));
#11448=CARTESIAN_POINT('Ctrl Pts',(98.4020470010275,-1.62605573728272,-1.48969924117991));
#11449=CARTESIAN_POINT('Ctrl Pts',(98.4061055276963,-1.57344374299025,-1.54333754818731));
#11450=CARTESIAN_POINT('Ctrl Pts',(98.4101682047153,-1.5207779463644,-1.597030707061));
#11451=CARTESIAN_POINT('Ctrl Pts',(98.4142308817344,-1.46538373010052,-1.64800151418336));
#11452=CARTESIAN_POINT('Ctrl Pts',(98.4182935587534,-1.40758181278408,-1.69597448103428));
#11453=CARTESIAN_POINT('Ctrl Pts',(98.4223583577632,-1.34974970475159,-1.7439725048087));
#11454=CARTESIAN_POINT('Ctrl Pts',(98.4264231567729,-1.28950777421597,-1.78896928415809));
#11455=CARTESIAN_POINT('Ctrl Pts',(98.4304879557826,-1.22720753181922,-1.83073145869245));
#11456=CARTESIAN_POINT('Ctrl Pts',(98.4345600160548,-1.16479599771715,-1.87256823620495));
#11457=CARTESIAN_POINT('Ctrl Pts',(98.438632076327,-1.10031921768597,-1.91115862178277));
#11458=CARTESIAN_POINT('Ctrl Pts',(98.4427041365992,-1.03415481414691,-1.94631441971146));
#11459=CARTESIAN_POINT('Ctrl Pts',(98.4458422870607,-0.983164936879575,
-1.97340738399038));
#11460=CARTESIAN_POINT('Ctrl Pts',(98.4489804375223,-0.931173316964451,
-1.99846144315086));
#11461=CARTESIAN_POINT('Ctrl Pts',(98.4521185879838,-0.878360093452682,
-2.02141028646581));
#11462=CARTESIAN_POINT('Ctrl Pts',(98.4561916533852,-0.809812802282947,
-2.0511960283713));
#11463=CARTESIAN_POINT('Ctrl Pts',(98.4602647187866,-0.739616525338188,
-2.07754853526234));
#11464=CARTESIAN_POINT('Ctrl Pts',(98.4643377841881,-0.668148923568016,
-2.10028403220491));
#11465=CARTESIAN_POINT('Ctrl Pts',(98.4684048654609,-0.5967863216628,-2.12298612626212));
#11466=CARTESIAN_POINT('Ctrl Pts',(98.4724719467337,-0.524156554541037,
-2.14208161747396));
#11467=CARTESIAN_POINT('Ctrl Pts',(98.4765390280066,-0.450657981229541,
-2.15743444487987));
#11468=CARTESIAN_POINT('Ctrl Pts',(98.4806013508446,-0.377245400341508,
-2.17276930966724));
#11469=CARTESIAN_POINT('Ctrl Pts',(98.4846636736825,-0.302966497826674,
-2.1843701133278));
#11470=CARTESIAN_POINT('Ctrl Pts',(98.4887259965205,-0.228233966287282,
-2.19215082889677));
#11471=CARTESIAN_POINT('Ctrl Pts',(98.4927857411294,-0.153548865143528,
-2.19992660628941));
#11472=CARTESIAN_POINT('Ctrl Pts',(98.4968454857384,-0.078411179979942,
-2.20388705741142));
#11473=CARTESIAN_POINT('Ctrl Pts',(98.5009052303474,-0.00324161999589336,
-2.20399761612843));
#11474=CARTESIAN_POINT('Ctrl Pts',(98.504963710272,0.0719045233018444,-2.20410814040439));
#11475=CARTESIAN_POINT('Ctrl Pts',(98.5090221901966,0.147082044556721,-2.20037115275537));
#11476=CARTESIAN_POINT('Ctrl Pts',(98.5130806701213,0.221868932772679,-2.19280418110471));
#11477=CARTESIAN_POINT('Ctrl Pts',(98.5171391972225,0.29665669032631,-2.18523712149407));
#11478=CARTESIAN_POINT('Ctrl Pts',(98.5211977243237,0.371053330970389,-2.17384003933285));
#11479=CARTESIAN_POINT('Ctrl Pts',(98.5252562514249,0.444642282234361,-2.15868229270762));
#11480=CARTESIAN_POINT('Ctrl Pts',(98.5293189288743,0.51830648734473,-2.14350904540305));
#11481=CARTESIAN_POINT('Ctrl Pts',(98.5333816063238,0.591160884992382,-2.1245675504363));
#11482=CARTESIAN_POINT('Ctrl Pts',(98.5374442837732,0.66280015669062,-2.10197810461738));
#11483=CARTESIAN_POINT('Ctrl Pts',(98.5415090832129,0.7344768465289,-2.07937686003186));
#11484=CARTESIAN_POINT('Ctrl Pts',(98.5455738826526,0.804936698691908,-2.0531240370874));
#11485=CARTESIAN_POINT('Ctrl Pts',(98.5496386820922,0.873793119374038,-2.02338863902479));
#11486=CARTESIAN_POINT('Ctrl Pts',(98.5537107427888,0.942772543457405,-1.99360012238496));
#11487=CARTESIAN_POINT('Ctrl Pts',(98.5577828034853,1.01014238607789,-1.96031681608829));
#11488=CARTESIAN_POINT('Ctrl Pts',(98.5618548641818,1.0755398661799,-1.92375414132308));
#11489=CARTESIAN_POINT('Ctrl Pts',(98.5649930107888,1.12593864350324,-1.89557699900869));
#11490=CARTESIAN_POINT('Ctrl Pts',(98.5681311573959,1.17516650040913,-1.86545318199277));
#11491=CARTESIAN_POINT('Ctrl Pts',(98.5712693040029,1.2230701006524,-1.83349816713574));
#11492=CARTESIAN_POINT('Ctrl Pts',(98.5753423677599,1.28524514930769,-1.792023109031));
#11493=CARTESIAN_POINT('Ctrl Pts',(98.5794154315169,1.34542804035084,-1.74730189288413));
#11494=CARTESIAN_POINT('Ctrl Pts',(98.5834884952739,1.40325968770601,-1.69955236720121));
#11495=CARTESIAN_POINT('Ctrl Pts',(98.5875555749001,1.4610063690102,-1.65187299495191));
#11496=CARTESIAN_POINT('Ctrl Pts',(98.5916226545262,1.51640829997285,-1.60117444807728));
#11497=CARTESIAN_POINT('Ctrl Pts',(98.5956897341524,1.56913528317269,-1.54771782412124));
#11498=CARTESIAN_POINT('Ctrl Pts',(98.5997520553481,1.62180057648512,-1.49432374372283));
#11499=CARTESIAN_POINT('Ctrl Pts',(98.6038143765438,1.67179680634006,-1.43817833560501));
#11500=CARTESIAN_POINT('Ctrl Pts',(98.6078766977395,1.71882806235913,-1.37958185405824));
#11501=CARTESIAN_POINT('Ctrl Pts',(98.6119364407097,1.76582946914223,-1.32102256182668));
#11502=CARTESIAN_POINT('Ctrl Pts',(98.6159961836799,1.8098693381602,-1.26001565453461));
#11503=CARTESIAN_POINT('Ctrl Pts',(98.6200559266501,1.85069066799873,-1.19689600692058));
#11504=CARTESIAN_POINT('Ctrl Pts',(98.6241144049417,1.89149928130278,-1.13379602214405));
#11505=CARTESIAN_POINT('Ctrl Pts',(98.6281728832333,1.92909108698606,-1.06858500444347));
#11506=CARTESIAN_POINT('Ctrl Pts',(98.6322313615249,1.96325216304356,-1.00162714834652));
#11507=CARTESIAN_POINT('Ctrl Pts',(98.6362898870011,1.99741363626414,-0.934668513784985));
#11508=CARTESIAN_POINT('Ctrl Pts',(98.6403484124774,2.02814408527399,-0.865963426624388));
#11509=CARTESIAN_POINT('Ctrl Pts',(98.6444069379536,2.05527609772403,-0.795899592991663));
#11510=CARTESIAN_POINT('Ctrl Pts',(98.6484696138018,2.08243585619754,-0.725764109945683));
#11511=CARTESIAN_POINT('Ctrl Pts',(98.6525322896499,2.10598965681717,-0.654267551915746));
#11512=CARTESIAN_POINT('Ctrl Pts',(98.6565949654981,2.12581899857559,-0.581815765767015));
#11513=CARTESIAN_POINT('Ctrl Pts',(98.6606597633471,2.14565869751758,-0.509326136887162));
#11514=CARTESIAN_POINT('Ctrl Pts',(98.6647245611961,2.16176996123382,-0.43588075312185));
#11515=CARTESIAN_POINT('Ctrl Pts',(98.6687893590451,2.17408537160911,-0.361896113484658));
#11516=CARTESIAN_POINT('Ctrl Pts',(98.6728614181864,2.18642278204383,-0.287779308826521));
#11517=CARTESIAN_POINT('Ctrl Pts',(98.6769334773277,2.19495074064123,-0.213121799223034));
#11518=CARTESIAN_POINT('Ctrl Pts',(98.6810055364689,2.19965374554041,-0.138345219397123));
#11519=CARTESIAN_POINT('Ctrl Pts',(98.6841436976533,2.20327814953667,-0.0807181191586382));
#11520=CARTESIAN_POINT('Ctrl Pts',(98.6872818588377,2.20463193494392,-0.02302042152449));
#11521=CARTESIAN_POINT('Ctrl Pts',(98.6904200200221,2.20372907897158,0.0345564248014581));
#11522=CARTESIAN_POINT('Ctrl Pts',(98.6944930856565,2.20255724890371,0.109286261901794));
#11523=CARTESIAN_POINT('Ctrl Pts',(98.6985661512908,2.19757764677268,0.184100536604629));
#11524=CARTESIAN_POINT('Ctrl Pts',(98.7026392169252,2.1887788129006,0.258579404047292));
#11525=CARTESIAN_POINT('Ctrl Pts',(98.7067062984189,2.17999290625919,0.332948847273765));
#11526=CARTESIAN_POINT('Ctrl Pts',(98.7107733799127,2.16739896396685,0.40698339138202));
#11527=CARTESIAN_POINT('Ctrl Pts',(98.7148404614064,2.15103752937728,0.48026403905611));
#11528=CARTESIAN_POINT('Ctrl Pts',(98.7189027844465,2.13469523753883,0.553458948942818));
#11529=CARTESIAN_POINT('Ctrl Pts',(98.7229651074865,2.11459431448589,0.625901251187874));
#11530=CARTESIAN_POINT('Ctrl Pts',(98.7270274305266,2.09082679201224,0.697179550620779));
#11531=CARTESIAN_POINT('Ctrl Pts',(98.7310871753261,2.0670743541073,0.768412611749784));
#11532=CARTESIAN_POINT('Ctrl Pts',(98.7351469201255,2.03966008528233,0.838482684259335));
#11533=CARTESIAN_POINT('Ctrl Pts',(98.739206664925,2.00872619729104,0.90699231767236));
#11534=CARTESIAN_POINT('Ctrl Pts',(98.7432651450284,1.97780194585806,0.975480608890158));
#11535=CARTESIAN_POINT('Ctrl Pts',(98.7473236251317,1.94336044854155,1.04240899128766));
#11536=CARTESIAN_POINT('Ctrl Pts',(98.7513821052351,1.90559190151686,1.10740033631625));
#11537=CARTESIAN_POINT('Ctrl Pts',(98.7554406325031,1.86782291557415,1.17239243662603));
#11538=CARTESIAN_POINT('Ctrl Pts',(98.7594991597712,1.82672704460385,1.23544704295642));
#11539=CARTESIAN_POINT('Ctrl Pts',(98.7635576870392,1.7825394460346,1.29621337878093));
#11540=CARTESIAN_POINT('Ctrl Pts',(98.767620364636,1.73830666036864,1.35704185544093));
#11541=CARTESIAN_POINT('Ctrl Pts',(98.7716830422329,1.69097611487498,1.41557700167304));
#11542=CARTESIAN_POINT('Ctrl Pts',(98.7757457198297,1.6408247153413,1.47149932161899));
#11543=CARTESIAN_POINT('Ctrl Pts',(98.7798105194062,1.59064712119879,1.52745085038681));
#11544=CARTESIAN_POINT('Ctrl Pts',(98.7838753189827,1.53764607582393,1.58078649619607));
#11545=CARTESIAN_POINT('Ctrl Pts',(98.7879401185593,1.48213511584823,1.63122392649494));
#11546=CARTESIAN_POINT('Ctrl Pts',(98.792012179374,1.42652499272933,1.68175145673308));
#11547=CARTESIAN_POINT('Ctrl Pts',(98.7960842401887,1.36839636919061,1.72937012721333));
#11548=CARTESIAN_POINT('Ctrl Pts',(98.8001563010034,1.3080952277046,1.77383845804979));
#11549=CARTESIAN_POINT('Ctrl Pts',(98.803294446016,1.26162398500473,1.80810810110852));
#11550=CARTESIAN_POINT('Ctrl Pts',(98.8064325910286,1.21386315119932,1.84050757261451));
#11551=CARTESIAN_POINT('Ctrl Pts',(98.8095707360412,1.16498120820677,1.87094489083059));
#11552=CARTESIAN_POINT('Ctrl Pts',(98.813757197885,1.09976994857186,1.91154998423045));
#11553=CARTESIAN_POINT('Ctrl Pts',(98.8179436597288,1.03232269390181,1.94881103154898));
#11554=CARTESIAN_POINT('Ctrl Pts',(98.8221301215726,0.963005805721677,1.98248223652732));
#11555=CARTESIAN_POINT('Ctrl Pts',(98.8263092907943,0.893809664342735,2.01609478782976));
#11556=CARTESIAN_POINT('Ctrl Pts',(98.8304884600159,0.82275075711108,2.04612973507325));
#11557=CARTESIAN_POINT('Ctrl Pts',(98.8346676292375,0.750222616012183,2.07238558825906));
#11558=CARTESIAN_POINT('Ctrl Pts',(98.8388389852493,0.677830070664218,2.0985923545377));
#11559=CARTESIAN_POINT('Ctrl Pts',(98.843010341261,0.603974171398295,2.12103393939962));
#11560=CARTESIAN_POINT('Ctrl Pts',(98.8471816972727,0.529069616147168,2.13955634215832));
#11561=CARTESIAN_POINT('Ctrl Pts',(98.8513484326716,0.454248032705071,2.15805822764328));
#11562=CARTESIAN_POINT('Ctrl Pts',(98.8555151680704,0.378380528606072,2.17264945329948));
#11563=CARTESIAN_POINT('Ctrl Pts',(98.8596819034693,0.301897734824081,2.18322553981674));
#11564=CARTESIAN_POINT('Ctrl Pts',(98.8638443463035,0.225493733501853,2.19379073086549));
#11565=CARTESIAN_POINT('Ctrl Pts',(98.8680067891378,0.148476140120422,2.20034895303591));
#11566=CARTESIAN_POINT('Ctrl Pts',(98.8721692319721,0.0712852104429588,
2.20284688954364));
#11567=CARTESIAN_POINT('Ctrl Pts',(98.8734622902489,0.0473059332520479,
2.20362287076546));
#11568=CARTESIAN_POINT('Ctrl Pts',(98.8747553485257,0.0233099826406988,
2.20400739829569));
#11569=CARTESIAN_POINT('Ctrl Pts',(98.8760484068025,-0.00068932936029577,
2.20399989220168));
#11570=CARTESIAN_POINT('',(99.6260484068026,-0.00167252030352725,2.20399936539824));
#11571=CARTESIAN_POINT('Ctrl Pts',(98.8760484068365,-0.000689329991730441,
2.20399989220149));
#11572=CARTESIAN_POINT('Ctrl Pts',(98.8804378272718,-0.0821574837625145,
2.2039744119635));
#11573=CARTESIAN_POINT('Ctrl Pts',(98.8848272477072,-0.163495403890133,
2.19942758819312));
#11574=CARTESIAN_POINT('Ctrl Pts',(98.8892166681425,-0.244213885737787,
2.19042817230167));
#11575=CARTESIAN_POINT('Ctrl Pts',(98.893604022686,-0.324894377228526,2.181432992008));
#11576=CARTESIAN_POINT('Ctrl Pts',(98.8979913772296,-0.404955679669053,
2.1679895597763));
#11577=CARTESIAN_POINT('Ctrl Pts',(98.9023787317731,-0.483923865789736,
2.15021712673839));
#11578=CARTESIAN_POINT('Ctrl Pts',(98.9067839458555,-0.563213506530593,
2.13237234772178));
#11579=CARTESIAN_POINT('Ctrl Pts',(98.9111891599379,-0.641400782654518,
2.11016339615855));
#11580=CARTESIAN_POINT('Ctrl Pts',(98.9155943740203,-0.718025682717486,
2.08375985155634));
#11581=CARTESIAN_POINT('Ctrl Pts',(98.9199700667003,-0.794137083444975,
2.05753324947015));
#11582=CARTESIAN_POINT('Ctrl Pts',(98.9243457593804,-0.868706716711618,
2.02716833620499));
#11583=CARTESIAN_POINT('Ctrl Pts',(98.9287214520604,-0.941307554494785,
1.99287633531312));
#11584=CARTESIAN_POINT('Ctrl Pts',(98.9327945073845,-1.00888707858082,1.96095608244838));
#11585=CARTESIAN_POINT('Ctrl Pts',(98.9368675627086,-1.07497143834343,1.9255328876901));
#11586=CARTESIAN_POINT('Ctrl Pts',(98.9409406180326,-1.13917351153671,1.88676964958977));
#11587=CARTESIAN_POINT('Ctrl Pts',(98.9450076892201,-1.20328125898522,1.84806336247438));
#11588=CARTESIAN_POINT('Ctrl Pts',(98.9490747604075,-1.26551180507766,1.80602701953534));
#11589=CARTESIAN_POINT('Ctrl Pts',(98.953141831595,-1.32550026940888,1.76087053351375));
#11590=CARTESIAN_POINT('Ctrl Pts',(98.957204144383,-1.38541854832619,1.71576687976078));
#11591=CARTESIAN_POINT('Ctrl Pts',(98.961266457171,-1.44309957762212,1.66755062136221));
#11592=CARTESIAN_POINT('Ctrl Pts',(98.965328769959,-1.49820665835499,1.61647542785554));
#11593=CARTESIAN_POINT('Ctrl Pts',(98.9693885045446,-1.55327876462395,1.56543264992032));
#11594=CARTESIAN_POINT('Ctrl Pts',(98.9734482391301,-1.60577981471814,1.51153486122198));
#11595=CARTESIAN_POINT('Ctrl Pts',(98.9775079737156,-1.65540652773743,1.45507567773099));
#11596=CARTESIAN_POINT('Ctrl Pts',(98.9815664436573,-1.70501778158834,1.39863408178452));
#11597=CARTESIAN_POINT('Ctrl Pts',(98.9856249135989,-1.7517561610921,1.33963303362135));
#11598=CARTESIAN_POINT('Ctrl Pts',(98.9896833835405,-1.79535670531577,1.27840146303018));
#11599=CARTESIAN_POINT('Ctrl Pts',(98.9937419007131,-1.8389577569464,1.2171691798487));
#11600=CARTESIAN_POINT('Ctrl Pts',(98.9978004178857,-1.87942062530542,1.15370671267549));
#11601=CARTESIAN_POINT('Ctrl Pts',(99.0018589350582,-1.91652291347563,1.08837306201638));
#11602=CARTESIAN_POINT('Ctrl Pts',(99.0059216027317,-1.95366314483411,1.02297259696035));
#11603=CARTESIAN_POINT('Ctrl Pts',(99.0099842704053,-1.98743569671596,0.955697543191284));
#11604=CARTESIAN_POINT('Ctrl Pts',(99.0140469380788,-2.01766389872753,0.886932010794298));
#11605=CARTESIAN_POINT('Ctrl Pts',(99.0181117278117,-2.04790788988244,0.818130559990831));
#11606=CARTESIAN_POINT('Ctrl Pts',(99.0221765175447,-2.07460367475865,0.747837526978033));
#11607=CARTESIAN_POINT('Ctrl Pts',(99.0262413072777,-2.09762355455813,0.676455041642015));
#11608=CARTESIAN_POINT('Ctrl Pts',(99.030313358491,-2.12068455786344,0.604945036176564));
#11609=CARTESIAN_POINT('Ctrl Pts',(99.0343854097043,-2.14005641622013,0.532342152943204));
#11610=CARTESIAN_POINT('Ctrl Pts',(99.0384574609176,-2.15566203483824,0.459061206765558));
#11611=CARTESIAN_POINT('Ctrl Pts',(99.0415956966382,-2.16768892429142,0.402585275867206));
#11612=CARTESIAN_POINT('Ctrl Pts',(99.0447339323588,-2.17747992202309,0.345706889448446));
#11613=CARTESIAN_POINT('Ctrl Pts',(99.0478721680795,-2.18502081063902,0.288617492668778));
#11614=CARTESIAN_POINT('Ctrl Pts',(99.0519452411864,-2.1948080265649,0.214521947459351));
#11615=CARTESIAN_POINT('Ctrl Pts',(99.0560183142934,-2.2008408984806,0.139785114427793));
#11616=CARTESIAN_POINT('Ctrl Pts',(99.0600913874004,-2.20304659179242,0.0648206324546741));
#11617=CARTESIAN_POINT('Ctrl Pts',(99.0641584763078,-2.20524904447765,-0.0100337109549575));
#11618=CARTESIAN_POINT('Ctrl Pts',(99.0682255652152,-2.20363546844268,-0.0851145659680157));
#11619=CARTESIAN_POINT('Ctrl Pts',(99.0722926541226,-2.19818459535836,-0.160001514771584));
#11620=CARTESIAN_POINT('Ctrl Pts',(99.0763549844544,-2.19274009990489,-0.234800844343007));
#11621=CARTESIAN_POINT('Ctrl Pts',(99.0804173147862,-2.18346726192895,-0.309406244646234));
#11622=CARTESIAN_POINT('Ctrl Pts',(99.084479645118,-2.17039685972843,-0.383397276047933));
#11623=CARTESIAN_POINT('Ctrl Pts',(99.0885393971312,-2.15733475317543,-0.45734134611617));
#11624=CARTESIAN_POINT('Ctrl Pts',(99.0925991491445,-2.14047994817327,-0.530671352076355));
#11625=CARTESIAN_POINT('Ctrl Pts',(99.0966589011577,-2.11991490433368,-0.602973298234623));
#11626=CARTESIAN_POINT('Ctrl Pts',(99.1007173883874,-2.09935626737051,-0.675252719294549));
#11627=CARTESIAN_POINT('Ctrl Pts',(99.1047758756171,-2.07508981708984,-0.746504257519102));
#11628=CARTESIAN_POINT('Ctrl Pts',(99.1088343628468,-2.04724845670253,-0.816326991180082));
#11629=CARTESIAN_POINT('Ctrl Pts',(99.1128928971441,-2.0194067734298,-0.886150534598268));
#11630=CARTESIAN_POINT('Ctrl Pts',(99.1169514314414,-1.98799027623994,-0.954544797714794));
#11631=CARTESIAN_POINT('Ctrl Pts',(99.1210099657387,-1.95318020468243,-1.02112834062947));
#11632=CARTESIAN_POINT('Ctrl Pts',(99.1250726501671,-1.91833453742703,-1.08777996980689));
#11633=CARTESIAN_POINT('Ctrl Pts',(99.1291353345954,-1.88008858778585,-1.15261675720722));
#11634=CARTESIAN_POINT('Ctrl Pts',(99.1331980190238,-1.83866947535711,-1.21528209087027));
#11635=CARTESIAN_POINT('Ctrl Pts',(99.137262825333,-1.79722873033025,-1.27798015372281));
#11636=CARTESIAN_POINT('Ctrl Pts',(99.1413276316422,-1.75261180574522,-1.33850411967357));
#11637=CARTESIAN_POINT('Ctrl Pts',(99.1453924379514,-1.70508750065945,-1.39652877345758));
#11638=CARTESIAN_POINT('Ctrl Pts',(99.1494645052614,-1.65747830247203,-1.45465707721232));
#11639=CARTESIAN_POINT('Ctrl Pts',(99.1535365725714,-1.60695167173138,-1.51027679728771));
#11640=CARTESIAN_POINT('Ctrl Pts',(99.1576086398813,-1.55381448750771,-1.56309837771369));
#11641=CARTESIAN_POINT('Ctrl Pts',(99.1607467212871,-1.51286506376914,-1.60380458582399));
#11642=CARTESIAN_POINT('Ctrl Pts',(99.1638848026929,-1.47036607962651,-1.64284976010869));
#11643=CARTESIAN_POINT('Ctrl Pts',(99.1670228840986,-1.42647071631425,-1.68011823854689));
#11644=CARTESIAN_POINT('Ctrl Pts',(99.1710959695303,-1.36949655226152,-1.72849101061917));
#11645=CARTESIAN_POINT('Ctrl Pts',(99.1751690549619,-1.30994919752869,-1.7740557142029));
#11646=CARTESIAN_POINT('Ctrl Pts',(99.1792421403935,-1.24813685368431,-1.81652701451837));
#11647=CARTESIAN_POINT('Ctrl Pts',(99.1833092418649,-1.18641532124411,-1.85893591826094));
#11648=CARTESIAN_POINT('Ctrl Pts',(99.1873763433363,-1.12243579659121,-1.89826017360842));
#11649=CARTESIAN_POINT('Ctrl Pts',(99.1914434448077,-1.05654011831091,-1.93425411422583));
#11650=CARTESIAN_POINT('Ctrl Pts',(99.195505787998,-0.990721534286376,-1.97020594394712));
#11651=CARTESIAN_POINT('Ctrl Pts',(99.1995681311883,-0.92299166748019,-2.0028349722339));
#11652=CARTESIAN_POINT('Ctrl Pts',(99.2036304743786,-0.853720574479981,
-2.03193926599925));
#11653=CARTESIAN_POINT('Ctrl Pts',(99.2076902394239,-0.784493444018035,
-2.0610250888762));
#11654=CARTESIAN_POINT('Ctrl Pts',(99.2117500044693,-0.713727467424388,
-2.08659043175383));
#11655=CARTESIAN_POINT('Ctrl Pts',(99.2158097695146,-0.641815286916337,
-2.10848029098697));
#11656=CARTESIAN_POINT('Ctrl Pts',(99.21986826993,-0.569925507284941,-2.13036333145821));
#11657=CARTESIAN_POINT('Ctrl Pts',(99.2239267703454,-0.496890689104043,
-2.14857302253901));
#11658=CARTESIAN_POINT('Ctrl Pts',(99.2279852707609,-0.42311981713259,-2.16300384196369));
#11659=CARTESIAN_POINT('Ctrl Pts',(99.2320438183777,-0.349348087186561,
-2.17743482922259));
#11660=CARTESIAN_POINT('Ctrl Pts',(99.2361023659946,-0.27484075537111,-2.18808676766113));
#11661=CARTESIAN_POINT('Ctrl Pts',(99.2401609136114,-0.200016621497414,
-2.19490531712071));
#11662=CARTESIAN_POINT('Ctrl Pts',(99.2442236114712,-0.125115972977261,
-2.20173083918223));
#11663=CARTESIAN_POINT('Ctrl Pts',(99.248286309331,-0.0498983520112227,
-2.20471510082763));
#11664=CARTESIAN_POINT('Ctrl Pts',(99.2523490071908,0.0252134507354692,
-2.20385577611195));
#11665=CARTESIAN_POINT('Ctrl Pts',(99.2564138270146,0.100364484688543,-2.20299600256741));
#11666=CARTESIAN_POINT('Ctrl Pts',(99.2604786468384,0.175409113396773,-2.19828867479555));
#11667=CARTESIAN_POINT('Ctrl Pts',(99.2645434666621,0.249928352263751,-2.18978350955859));
#11668=CARTESIAN_POINT('Ctrl Pts',(99.2686155474668,0.324580704722417,-2.18126315155919));
#11669=CARTESIAN_POINT('Ctrl Pts',(99.2726876282714,0.398705321071872,-2.16893148390978));
#11670=CARTESIAN_POINT('Ctrl Pts',(99.276759709076,0.471892555701658,-2.15288955031914));
#11671=CARTESIAN_POINT('Ctrl Pts',(99.2798976727566,0.528290966040015,-2.14052756454605));
#11672=CARTESIAN_POINT('Ctrl Pts',(99.2830356364372,0.584132908470223,-2.12596336727211));
#11673=CARTESIAN_POINT('Ctrl Pts',(99.2861736001177,0.639238193960531,-2.10926303039286));
#11674=CARTESIAN_POINT('Ctrl Pts',(99.2902465884069,0.710763299193751,-2.08758646448652));
#11675=CARTESIAN_POINT('Ctrl Pts',(99.294319576696,0.781322536814027,-2.06222583963422));
#11676=CARTESIAN_POINT('Ctrl Pts',(99.2983925649851,0.850509108205028,-2.03328558172734));
#11677=CARTESIAN_POINT('Ctrl Pts',(99.3024595690473,0.91959402741384,-2.00438784421583));
#11678=CARTESIAN_POINT('Ctrl Pts',(99.3065265731094,0.987309847693555,-1.97192109835214));
#11679=CARTESIAN_POINT('Ctrl Pts',(99.3105935771715,1.0532648847763,-1.93603953536522));
#11680=CARTESIAN_POINT('Ctrl Pts',(99.3146558230158,1.11914275733449,-1.90019995224626));
#11681=CARTESIAN_POINT('Ctrl Pts',(99.3187180688601,1.18326352219853,-1.86095371655459));
#11682=CARTESIAN_POINT('Ctrl Pts',(99.3227803147044,1.24525696235485,-1.81850243269202));
#11683=CARTESIAN_POINT('Ctrl Pts',(99.3268399824895,1.30721105906302,-1.77607809006518));
#11684=CARTESIAN_POINT('Ctrl Pts',(99.3308996502746,1.36704011718689,-1.73045300470282));
#11685=CARTESIAN_POINT('Ctrl Pts',(99.3349593180597,1.42440112548946,-1.68187319192155));
#11686=CARTESIAN_POINT('Ctrl Pts',(99.3390177214372,1.48174426836611,-1.63330850961082));
#11687=CARTESIAN_POINT('Ctrl Pts',(99.3430761248147,1.53662052349016,-1.58179123541503));
#11688=CARTESIAN_POINT('Ctrl Pts',(99.3471345281923,1.58871961326095,-1.52760793086445));
#11689=CARTESIAN_POINT('Ctrl Pts',(99.3511929791303,1.64081931358217,-1.47342399133849));
#11690=CARTESIAN_POINT('Ctrl Pts',(99.3552514300683,1.69014145427682,-1.41657430485035));
#11691=CARTESIAN_POINT('Ctrl Pts',(99.3593098810064,1.73641345784783,-1.3573814141224));
#11692=CARTESIAN_POINT('Ctrl Pts',(99.3633724834128,1.78273279395095,-1.29812797383567));
#11693=CARTESIAN_POINT('Ctrl Pts',(99.3674350858192,1.82599546766183,-1.23652691983741));
#11694=CARTESIAN_POINT('Ctrl Pts',(99.3714976882256,1.86597045674903,-1.17293233161159));
#11695=CARTESIAN_POINT('Ctrl Pts',(99.375562413125,1.90596633063594,-1.10930451860528));
#11696=CARTESIAN_POINT('Ctrl Pts',(99.3796271380245,1.94267086609419,-1.04368151441209));
#11697=CARTESIAN_POINT('Ctrl Pts',(99.383691862924,1.97589884494488,-0.976442396941821));
#11698=CARTESIAN_POINT('Ctrl Pts',(99.3877638507495,2.00918619616578,-0.909083135366692));
#11699=CARTESIAN_POINT('Ctrl Pts',(99.3918358385749,2.03898439321521,-0.840102431539732));
#11700=CARTESIAN_POINT('Ctrl Pts',(99.3959078264004,2.06515641817133,-0.769899323603909));
#11701=CARTESIAN_POINT('Ctrl Pts',(99.3990466563126,2.08533072573685,-0.715784325092066));
#11702=CARTESIAN_POINT('Ctrl Pts',(99.4021854862248,2.1033513993086,-0.660943415302023));
#11703=CARTESIAN_POINT('Ctrl Pts',(99.4053243161369,2.11917631141579,-0.605564002508532));
#11704=CARTESIAN_POINT('Ctrl Pts',(99.4093974652079,2.13971174272361,-0.533700088220429));
#11705=CARTESIAN_POINT('Ctrl Pts',(99.4134706142789,2.15662713355787,-0.460651852012233));
#11706=CARTESIAN_POINT('Ctrl Pts',(99.41754376335,2.16978984641977,-0.386817815481237));
#11707=CARTESIAN_POINT('Ctrl Pts',(99.4216109278203,2.18293321955733,-0.313092261899616));
#11708=CARTESIAN_POINT('Ctrl Pts',(99.4256780922906,2.19233477865686,-0.238583666401459));
#11709=CARTESIAN_POINT('Ctrl Pts',(99.429745256761,2.19791190347919,-0.163704809167205));
#11710=CARTESIAN_POINT('Ctrl Pts',(99.4338076617085,2.20348250177602,-0.0889135775083088));
#11711=CARTESIAN_POINT('Ctrl Pts',(99.4378700666561,2.20523752226794,-0.0137534186954298));
#11712=CARTESIAN_POINT('Ctrl Pts',(99.4419324716036,2.20314582682219,0.0613552422859288));
#11713=CARTESIAN_POINT('Ctrl Pts',(99.445992297618,2.20105545924574,0.136416222098011));
#11714=CARTESIAN_POINT('Ctrl Pts',(99.4500521236324,2.19512323489591,0.211425292907891));
#11715=CARTESIAN_POINT('Ctrl Pts',(99.4541119496467,2.18537008339007,0.285960834072956));
#11716=CARTESIAN_POINT('Ctrl Pts',(99.4581705101639,2.17561997206034,0.360473141601971));
#11717=CARTESIAN_POINT('Ctrl Pts',(99.4622290706811,2.16205136022153,0.434511739454726));
#11718=CARTESIAN_POINT('Ctrl Pts',(99.4662876311982,2.14473699205026,0.507660550891255));
#11719=CARTESIAN_POINT('Ctrl Pts',(99.4703462379696,2.127422426552,0.580810195984218));
#11720=CARTESIAN_POINT('Ctrl Pts',(99.4744048447411,2.10636213167654,0.653069570337208));
#11721=CARTESIAN_POINT('Ctrl Pts',(99.4784634515125,2.081679520328,0.724034788285061));
#11722=CARTESIAN_POINT('Ctrl Pts',(99.482526206663,2.05697168041345,0.795072541130457));
#11723=CARTESIAN_POINT('Ctrl Pts',(99.4865889618135,2.0286342876539,0.864813044104926));
#11724=CARTESIAN_POINT('Ctrl Pts',(99.4906517169641,1.9968397770103,0.93287025086528));
#11725=CARTESIAN_POINT('Ctrl Pts',(99.4947165931353,1.96502866757765,1.00096298788527));
#11726=CARTESIAN_POINT('Ctrl Pts',(99.4987814693065,1.92975707025435,1.06737025661494));
#11727=CARTESIAN_POINT('Ctrl Pts',(99.5028463454778,1.89124324927213,1.1317309627657));
#11728=CARTESIAN_POINT('Ctrl Pts',(99.5069184804549,1.85266065267633,1.19620660030846));
#11729=CARTESIAN_POINT('Ctrl Pts',(99.5109906154321,1.81082453401622,1.2586279782448));
#11730=CARTESIAN_POINT('Ctrl Pts',(99.5150627504093,1.76599605057846,1.31866369834817));
#11731=CARTESIAN_POINT('Ctrl Pts',(99.5182001776582,1.73145738566371,1.36491896867078));
#11732=CARTESIAN_POINT('Ctrl Pts',(99.5213376049071,1.69514330785048,1.40975868348756));
#11733=CARTESIAN_POINT('Ctrl Pts',(99.524475032156,1.65718831331425,1.45304607436057));
#11734=CARTESIAN_POINT('Ctrl Pts',(99.5284883777273,1.60863690569746,1.50841859607012));
#11735=CARTESIAN_POINT('Ctrl Pts',(99.5325017232986,1.55720003307881,1.56147683584796));
#11736=CARTESIAN_POINT('Ctrl Pts',(99.5365150688698,1.50313021226308,1.61189812487699));
#11737=CARTESIAN_POINT('Ctrl Pts',(99.5405215924509,1.44915230074844,1.66223370647506));
#11738=CARTESIAN_POINT('Ctrl Pts',(99.544528116032,1.39255068593022,1.70994090581197));
#11739=CARTESIAN_POINT('Ctrl Pts',(99.5485346396131,1.33361720663063,1.75473107517326));
#11740=CARTESIAN_POINT('Ctrl Pts',(99.5525373552304,1.2747397401197,1.79947867412602));
#11741=CARTESIAN_POINT('Ctrl Pts',(99.5565400708476,1.21353519271828,1.84131444273081));
#11742=CARTESIAN_POINT('Ctrl Pts',(99.5605427864649,1.15033023490278,1.8799883910994));
#11743=CARTESIAN_POINT('Ctrl Pts',(99.5645430802893,1.08716351845349,1.91863894028107));
#11744=CARTESIAN_POINT('Ctrl Pts',(99.5685433741137,1.02199921149075,1.95413120698742));
#11745=CARTESIAN_POINT('Ctrl Pts',(99.5725436679381,0.955193379403557,1.98625819266872));
#11746=CARTESIAN_POINT('Ctrl Pts',(99.5765429227281,0.888404899432113,2.01837683370171));
#11747=CARTESIAN_POINT('Ctrl Pts',(99.580542177518,0.819976185039759,2.0471317165054));
#11748=CARTESIAN_POINT('Ctrl Pts',(99.584541432308,0.750286714981923,2.0723623827221));
#11749=CARTESIAN_POINT('Ctrl Pts',(99.5885430400031,0.680556244106896,2.09760789304557));
#11750=CARTESIAN_POINT('Ctrl Pts',(99.5925446476982,0.609563999543172,2.11932487609767));
#11751=CARTESIAN_POINT('Ctrl Pts',(99.5965462553934,0.53770706366451,2.13740195416896));
#11752=CARTESIAN_POINT('Ctrl Pts',(99.6005491822716,0.465826439193568,2.15548499158888));
#11753=CARTESIAN_POINT('Ctrl Pts',(99.6045521091498,0.393081039035946,2.16992563667628));
#11754=CARTESIAN_POINT('Ctrl Pts',(99.608555036028,0.319878123329642,2.18066365728764));
#11755=CARTESIAN_POINT('Ctrl Pts',(99.6125632404791,0.246578694811779,2.19141583521158));
#11756=CARTESIAN_POINT('Ctrl Pts',(99.6165714449303,0.172821037268198,2.19845559879149));
#11757=CARTESIAN_POINT('Ctrl Pts',(99.6205796493814,0.0990164677374564,
2.20177467946127));
#11758=CARTESIAN_POINT('Ctrl Pts',(99.6224025685218,0.0654503749680512,
2.20328418721099));
#11759=CARTESIAN_POINT('Ctrl Pts',(99.6242254876622,0.0318745667734997,
2.20402482283944));
#11760=CARTESIAN_POINT('Ctrl Pts',(99.6260484068026,-0.00167252030352725,
2.20399936539824));
#11761=CARTESIAN_POINT('',(100.349820515151,0.480300475185355,2.15472339387338));
#11762=CARTESIAN_POINT('Ctrl Pts',(99.6260484068026,-0.00167396307086296,
2.20590060288082));
#11763=CARTESIAN_POINT('Ctrl Pts',(99.6319075205934,-0.109592698905016,
2.20681139051173));
#11764=CARTESIAN_POINT('Ctrl Pts',(99.6774835397241,-0.948102371469299,
2.15053535437817));
#11765=CARTESIAN_POINT('Ctrl Pts',(99.7627764641942,-2.37345450507347,1.07511981627215));
#11766=CARTESIAN_POINT('Ctrl Pts',(99.8819271802135,-2.18961305998529,-1.41221794055659));
#11767=CARTESIAN_POINT('Ctrl Pts',(100.001077896233,0.000573147000856311,
-2.6057943353733));
#11768=CARTESIAN_POINT('Ctrl Pts',(100.120228612252,2.19048665599282,-1.41085615541611));
#11769=CARTESIAN_POINT('Ctrl Pts',(100.236476151891,2.36818650235432,1.01501035828337));
#11770=CARTESIAN_POINT('Ctrl Pts',(100.313006786191,1.14036460413367,2.00378250651846));
#11771=CARTESIAN_POINT('Ctrl Pts',(100.349820515151,0.480300475185355,2.15472339387338));
#11772=CARTESIAN_POINT('',(100.349869898682,1.9893770426062,0.948680653513814));
#11773=CARTESIAN_POINT('Origin',(100.349869898682,0.,0.));
#11774=CARTESIAN_POINT('',(99.7342548474101,-0.00178926204916046,2.20399927371615));
#11775=CARTESIAN_POINT('Ctrl Pts',(100.349869898682,1.9893770426062,0.948680653513813));
#11776=CARTESIAN_POINT('Ctrl Pts',(100.310152993343,2.30503304407864,0.286752110579726));
#11777=CARTESIAN_POINT('Ctrl Pts',(100.230719182663,2.21766422752178,-1.36580521532166));
#11778=CARTESIAN_POINT('Ctrl Pts',(100.111568466644,0.0501856098512207,
-2.6066853763117));
#11779=CARTESIAN_POINT('Ctrl Pts',(99.9924177506253,-2.1620698968013,-1.45316896147941));
#11780=CARTESIAN_POINT('Ctrl Pts',(99.8732670346058,-2.39365166732773,1.02916391750694));
#11781=CARTESIAN_POINT('Ctrl Pts',(99.7872127335343,-0.976535127098266,
2.14187097997843));
#11782=CARTESIAN_POINT('Ctrl Pts',(99.7408753378023,-0.12379021475703,2.20663616064201));
#11783=CARTESIAN_POINT('Ctrl Pts',(99.7342548474101,-0.00179052749946479,
2.20555804569826));
#11784=CARTESIAN_POINT('',(98.9842548474577,-0.000466138566021928,2.20399995070663));
#11785=CARTESIAN_POINT('Ctrl Pts',(99.7342548474101,-0.00178926204916046,
2.20399927371615));
#11786=CARTESIAN_POINT('Ctrl Pts',(99.7301177955417,0.0743921602789955,
2.20406111971104));
#11787=CARTESIAN_POINT('Ctrl Pts',(99.7259807436732,0.150715896488296,2.20016833951562));
#11788=CARTESIAN_POINT('Ctrl Pts',(99.7218436918048,0.226730373341687,2.19230685302134));
#11789=CARTESIAN_POINT('Ctrl Pts',(99.7178416649022,0.300263892144504,2.1847019494704));
#11790=CARTESIAN_POINT('Ctrl Pts',(99.7138396379996,0.373507490498452,2.17338344944699));
#11791=CARTESIAN_POINT('Ctrl Pts',(99.7098376110969,0.446051984251043,2.15839144442006));
#11792=CARTESIAN_POINT('Ctrl Pts',(99.7058380234803,0.51855226121741,2.14340857720976));
#11793=CARTESIAN_POINT('Ctrl Pts',(99.7018384358637,0.590353796805677,2.1247567438145));
#11794=CARTESIAN_POINT('Ctrl Pts',(99.6978388482471,0.661055196870396,2.10252753292095));
#11795=CARTESIAN_POINT('Ctrl Pts',(99.6938403161961,0.731737937518075,2.08030418873041));
#11796=CARTESIAN_POINT('Ctrl Pts',(99.6898417841452,0.801320648756876,2.05450548855933));
#11797=CARTESIAN_POINT('Ctrl Pts',(99.6858432520943,0.869416528199261,2.02527304344228));
#11798=CARTESIAN_POINT('Ctrl Pts',(99.6818443935192,0.937517968420832,1.99603821117385));
#11799=CARTESIAN_POINT('Ctrl Pts',(99.6778455349441,1.0041318842539,1.96336927512572));
#11800=CARTESIAN_POINT('Ctrl Pts',(99.6738466763689,1.06889260099549,1.92745547485204));
#11801=CARTESIAN_POINT('Ctrl Pts',(99.6698436806361,1.13372031817998,1.89150451871219));
#11802=CARTESIAN_POINT('Ctrl Pts',(99.6658406849033,1.1966905809756,1.85230224284687));
#11803=CARTESIAN_POINT('Ctrl Pts',(99.6618376891705,1.25746437939013,1.81008268721763));
#11804=CARTESIAN_POINT('Ctrl Pts',(99.6578321875143,1.31827622293191,1.76783670163982));
#11805=CARTESIAN_POINT('Ctrl Pts',(99.6538266858582,1.37688847994479,1.72256998339863));
#11806=CARTESIAN_POINT('Ctrl Pts',(99.649821184202,1.4329952624189,1.67455683029421));
#11807=CARTESIAN_POINT('Ctrl Pts',(99.6458092838468,1.48919167421968,1.62646697725452));
#11808=CARTESIAN_POINT('Ctrl Pts',(99.6417973834915,1.54287427675369,1.5756222814579));
#11809=CARTESIAN_POINT('Ctrl Pts',(99.6377854831363,1.59377480585921,1.52233303459146));
#11810=CARTESIAN_POINT('Ctrl Pts',(99.6368455229467,1.6057004437741,1.50984773681451));
#11811=CARTESIAN_POINT('Ctrl Pts',(99.6359055627572,1.61747354506083,1.49722838528258));
#11812=CARTESIAN_POINT('Ctrl Pts',(99.6349656025676,1.6290909969087,1.48447920961899));
#11813=CARTESIAN_POINT('Ctrl Pts',(99.630891816437,1.67944101676689,1.429224300346));
#11814=CARTESIAN_POINT('Ctrl Pts',(99.6268180303064,1.72707337135986,1.37129874505747));
#11815=CARTESIAN_POINT('Ctrl Pts',(99.6227442441758,1.77169212129934,1.31100077319804));
#11816=CARTESIAN_POINT('Ctrl Pts',(99.6186764265708,1.81624550007225,1.25079114421615));
#11817=CARTESIAN_POINT('Ctrl Pts',(99.6146086089659,1.85779375883192,1.18821638020305));
#11818=CARTESIAN_POINT('Ctrl Pts',(99.6105407913609,1.89607943995466,1.12360969975398));
#11819=CARTESIAN_POINT('Ctrl Pts',(99.6064777123138,1.93432052249017,1.0590782789474));
#11820=CARTESIAN_POINT('Ctrl Pts',(99.6024146332668,1.96930633614992,0.9925200528759));
#11821=CARTESIAN_POINT('Ctrl Pts',(99.5983515542198,2.00082215241775,0.924297957584244));
#11822=CARTESIAN_POINT('Ctrl Pts',(99.5942910415887,2.0323180619365,0.856118954310918));
#11823=CARTESIAN_POINT('Ctrl Pts',(99.5902305289577,2.06034812386471,0.786278599563272));
#11824=CARTESIAN_POINT('Ctrl Pts',(99.5861700163267,2.08474372803297,0.715164029036125));
#11825=CARTESIAN_POINT('Ctrl Pts',(99.5821107576639,2.10913179834626,0.64407142012377));
#11826=CARTESIAN_POINT('Ctrl Pts',(99.5780514990011,2.12988748463402,0.571705827876288));
#11827=CARTESIAN_POINT('Ctrl Pts',(99.5739922403383,2.14689106090511,0.498472439163638));
#11828=CARTESIAN_POINT('Ctrl Pts',(99.5699329248685,2.16389487513162,0.425238025591169));
#11829=CARTESIAN_POINT('Ctrl Pts',(99.5658736093987,2.17714636888608,0.351136256741012));
#11830=CARTESIAN_POINT('Ctrl Pts',(99.5618142939289,2.18657662602126,0.276583908674142));
#11831=CARTESIAN_POINT('Ctrl Pts',(99.5577508185871,2.19601654701804,0.201955161463279));
#11832=CARTESIAN_POINT('Ctrl Pts',(99.5536873432452,2.20162735158575,0.12687538750957));
#11833=CARTESIAN_POINT('Ctrl Pts',(99.5496238679034,2.20339196712703,0.0517671633382531));
#11834=CARTESIAN_POINT('Ctrl Pts',(99.5455582640324,2.205157507009,-0.0233804040138641));
#11835=CARTESIAN_POINT('Ctrl Pts',(99.5414926601615,2.20307285899171,-0.0985559737415544));
#11836=CARTESIAN_POINT('Ctrl Pts',(99.5374270562905,2.19717309413235,-0.173338958174133));
#11837=CARTESIAN_POINT('Ctrl Pts',(99.5333541895044,2.19126278975843,-0.248255537143437));
#11838=CARTESIAN_POINT('Ctrl Pts',(99.5292813227183,2.18152381717142,-0.322777656036424));
#11839=CARTESIAN_POINT('Ctrl Pts',(99.5252084559323,2.16804286873909,-0.396492268915249));
#11840=CARTESIAN_POINT('Ctrl Pts',(99.5220772661377,2.15767881551315,-0.45316351687983));
#11841=CARTESIAN_POINT('Ctrl Pts',(99.518946076343,2.14510416478066,-0.509357638457879));
#11842=CARTESIAN_POINT('Ctrl Pts',(99.5158148865484,2.1303782225379,-0.564893466891131));
#11843=CARTESIAN_POINT('Ctrl Pts',(99.5117423865472,2.11122531142885,-0.637124687672423));
#11844=CARTESIAN_POINT('Ctrl Pts',(99.507669886546,2.08835766175706,-0.708520398955298));
#11845=CARTESIAN_POINT('Ctrl Pts',(99.5035973865447,2.06186525068677,-0.778670461755417));
#11846=CARTESIAN_POINT('Ctrl Pts',(99.4995308792193,2.03541182314764,-0.848717298875088));
#11847=CARTESIAN_POINT('Ctrl Pts',(99.4954643718939,2.00534439126511,-0.917521683578741));
#11848=CARTESIAN_POINT('Ctrl Pts',(99.4913978645685,1.97180320036611,-0.984686822815248));
#11849=CARTESIAN_POINT('Ctrl Pts',(99.4873361257298,1.93830134069428,-1.05177320255399));
#11850=CARTESIAN_POINT('Ctrl Pts',(99.483274386891,1.90133402720749,-1.11722373067191));
#11851=CARTESIAN_POINT('Ctrl Pts',(99.4792126480523,1.86108964626999,-1.18066139453556));
#11852=CARTESIAN_POINT('Ctrl Pts',(99.4751534933172,1.82087086905829,-1.24405869896235));
#11853=CARTESIAN_POINT('Ctrl Pts',(99.471094338582,1.77737941679389,-1.30544527803626));
#11854=CARTESIAN_POINT('Ctrl Pts',(99.4670351838469,1.73084901870324,-1.36446974112804));
#11855=CARTESIAN_POINT('Ctrl Pts',(99.4629772988251,1.68433317543317,-1.42347574122564));
#11856=CARTESIAN_POINT('Ctrl Pts',(99.4589194138033,1.63478056916153,-1.48012071749539));
#11857=CARTESIAN_POINT('Ctrl Pts',(99.4548615287815,1.58246660369059,-1.53408456357659));
#11858=CARTESIAN_POINT('Ctrl Pts',(99.4508036007722,1.53015208402688,-1.58804898132871));
#11859=CARTESIAN_POINT('Ctrl Pts',(99.4467456727628,1.47507648081182,-1.63933187082003));
#11860=CARTESIAN_POINT('Ctrl Pts',(99.4426877447535,1.41755248405717,-1.68764953557999));
#11861=CARTESIAN_POINT('Ctrl Pts',(99.4386256687448,1.3599696864823,-1.73601659048109));
#11862=CARTESIAN_POINT('Ctrl Pts',(99.4345635927362,1.29993386406711,-1.78141205995232));
#11863=CARTESIAN_POINT('Ctrl Pts',(99.4305015167276,1.23779068576521,-1.82359266784907));
#11864=CARTESIAN_POINT('Ctrl Pts',(99.4264373209815,1.17561507891557,-1.86579528710563));
#11865=CARTESIAN_POINT('Ctrl Pts',(99.4223731252354,1.11133033503176,-1.90477945608713));
#11866=CARTESIAN_POINT('Ctrl Pts',(99.4183089294893,1.04530871568077,-1.94034679604493));
#11867=CARTESIAN_POINT('Ctrl Pts',(99.4142374693345,0.979169088228575,-1.97597770963655));
#11868=CARTESIAN_POINT('Ctrl Pts',(99.4101660091798,0.911286816445657,-2.00817939036449));
#11869=CARTESIAN_POINT('Ctrl Pts',(99.406094549025,0.842055802925244,-2.03680092909443));
#11870=CARTESIAN_POINT('Ctrl Pts',(99.4029510895265,0.788604490921365,-2.05889881151578));
#11871=CARTESIAN_POINT('Ctrl Pts',(99.3998076300279,0.734349660433825,-2.07886356027579));
#11872=CARTESIAN_POINT('Ctrl Pts',(99.3966641705294,0.679477986987283,-2.09664628995921));
#11873=CARTESIAN_POINT('Ctrl Pts',(99.3925909798832,0.608377090942739,-2.11968856177621));
#11874=CARTESIAN_POINT('Ctrl Pts',(99.3885177892369,0.535965708987452,-2.1391544187786));
#11875=CARTESIAN_POINT('Ctrl Pts',(99.3844445985907,0.462637481712026,-2.15489734338208));
#11876=CARTESIAN_POINT('Ctrl Pts',(99.3803773913427,0.389416971464416,-2.17061714208834));
#11877=CARTESIAN_POINT('Ctrl Pts',(99.3763101840948,0.315282752805154,-2.18262476699012));
#11878=CARTESIAN_POINT('Ctrl Pts',(99.3722429768469,0.240644467779498,-2.19082318778288));
#11879=CARTESIAN_POINT('Ctrl Pts',(99.3681805275575,0.166093497179889,-2.19901201778177));
#11880=CARTESIAN_POINT('Ctrl Pts',(99.3641180782681,0.0910401039530714,
-2.20340044515141));
#11881=CARTESIAN_POINT('Ctrl Pts',(99.3600556289787,0.0159033734873056,
-2.20394262237285));
#11882=CARTESIAN_POINT('Ctrl Pts',(99.3559957576903,-0.0591856757522623,
-2.20448445553255));
#11883=CARTESIAN_POINT('Ctrl Pts',(99.3519358864019,-0.134357481080633,
-2.20118487862807));
#11884=CARTESIAN_POINT('Ctrl Pts',(99.3478760151135,-0.209189938435319,
-2.19405003809335));
#11885=CARTESIAN_POINT('Ctrl Pts',(99.343817408466,-0.28399908564479,-2.1869174200457));
#11886=CARTESIAN_POINT('Ctrl Pts',(99.3397588018185,-0.358468619794764,
-2.17595195563659));
#11887=CARTESIAN_POINT('Ctrl Pts',(99.335700195171,-0.432180162262118,-2.16121176827887));
#11888=CARTESIAN_POINT('Ctrl Pts',(99.331641541488,-0.505892558978118,-2.14647141009601));
#11889=CARTESIAN_POINT('Ctrl Pts',(99.3275828878051,-0.57884647876335,-2.12795633748231));
#11890=CARTESIAN_POINT('Ctrl Pts',(99.3235242341221,-0.650633951486543,
-2.10577573857546));
#11891=CARTESIAN_POINT('Ctrl Pts',(99.3194614312018,-0.722494813881127,
-2.08357246402892));
#11892=CARTESIAN_POINT('Ctrl Pts',(99.3153986282815,-0.793186390734587,
-2.0576963212229));
#11893=CARTESIAN_POINT('Ctrl Pts',(99.3113358253612,-0.862316822649757,
-2.02830611530292));
#11894=CARTESIAN_POINT('Ctrl Pts',(99.3072709008695,-0.931483354063812,
-1.99890056199286));
#11895=CARTESIAN_POINT('Ctrl Pts',(99.3032059763777,-0.999086687470405,
-1.96597750051935));
#11896=CARTESIAN_POINT('Ctrl Pts',(99.299141051886,-1.06475829435055,-1.92974241146629));
#11897=CARTESIAN_POINT('Ctrl Pts',(99.2950688682582,-1.13054717748865,-1.89344261384505));
#11898=CARTESIAN_POINT('Ctrl Pts',(99.2909966846303,-1.19439703737409,-1.85381922677039));
#11899=CARTESIAN_POINT('Ctrl Pts',(99.2869245010025,-1.25596752021542,-1.81112163814691));
#11900=CARTESIAN_POINT('Ctrl Pts',(99.2837874855051,-1.3033984753269,-1.77822945806464));
#11901=CARTESIAN_POINT('Ctrl Pts',(99.2806504700076,-1.34947732050749,-1.74351382884607));
#11902=CARTESIAN_POINT('Ctrl Pts',(99.2775134545102,-1.39406271455528,-1.70710431663878));
#11903=CARTESIAN_POINT('Ctrl Pts',(99.2734403154914,-1.45195293164663,-1.65982976381973));
#11904=CARTESIAN_POINT('Ctrl Pts',(99.2693671764726,-1.50754729424262,-1.60951604503001));
#11905=CARTESIAN_POINT('Ctrl Pts',(99.2652940374537,-1.56050937957516,-1.55641462221927));
#11906=CARTESIAN_POINT('Ctrl Pts',(99.2612268808056,-1.61339367752509,-1.50339119144127));
#11907=CARTESIAN_POINT('Ctrl Pts',(99.2571597241573,-1.66365303969438,-1.44758852095762));
#11908=CARTESIAN_POINT('Ctrl Pts',(99.2530925675092,-1.71098396732507,-1.38929833497221));
#11909=CARTESIAN_POINT('Ctrl Pts',(99.2490301670178,-1.75825954589085,-1.33107631387285));
#11910=CARTESIAN_POINT('Ctrl Pts',(99.2449677665265,-1.80261319423376,-1.27037292540568));
#11911=CARTESIAN_POINT('Ctrl Pts',(99.2409053660352,-1.84377931595503,-1.20751556265599));
#11912=CARTESIAN_POINT('Ctrl Pts',(99.2368455424143,-1.88491932509632,-1.14469807171942));
#11913=CARTESIAN_POINT('Ctrl Pts',(99.2327857187933,-1.92287555898522,-1.07972971620207));
#11914=CARTESIAN_POINT('Ctrl Pts',(99.2287258951723,-1.95742448661696,-1.01296859733771));
#11915=CARTESIAN_POINT('Ctrl Pts',(99.2246673349892,-1.99196266244554,-0.946228254875343));
#11916=CARTESIAN_POINT('Ctrl Pts',(99.2206087748061,-2.023095418051,-0.877696680538174));
#11917=CARTESIAN_POINT('Ctrl Pts',(99.2165502146231,-2.05064492767362,-0.807757005916043));
#11918=CARTESIAN_POINT('Ctrl Pts',(99.2124916061278,-2.07819476523911,-0.737816498748508));
#11919=CARTESIAN_POINT('Ctrl Pts',(99.2084329976326,-2.10216109881843,-0.666468302891899));
#11920=CARTESIAN_POINT('Ctrl Pts',(99.2043743891374,-2.12241466213535,-0.5941144687288));
#11921=CARTESIAN_POINT('Ctrl Pts',(99.2003116290888,-2.14268894283582,-0.521686623780005));
#11922=CARTESIAN_POINT('Ctrl Pts',(99.1962488690402,-2.1592427403123,-0.448251547122586));
#11923=CARTESIAN_POINT('Ctrl Pts',(99.1921861089916,-2.17199722044688,-0.374224630898386));
#11924=CARTESIAN_POINT('Ctrl Pts',(99.1881212261541,-2.18475836478738,-0.300159035668188));
#11925=CARTESIAN_POINT('Ctrl Pts',(99.1840563433165,-2.1937161816409,-0.225501459539191));
#11926=CARTESIAN_POINT('Ctrl Pts',(99.179991460479,-2.19884370864308,-0.150672973557745));
#11927=CARTESIAN_POINT('Ctrl Pts',(99.1759193160121,-2.20398039561424,-0.075710811710773));
#11928=CARTESIAN_POINT('Ctrl Pts',(99.1718471715452,-2.20527311705613,-0.000577608238949548));
#11929=CARTESIAN_POINT('Ctrl Pts',(99.1677750270782,-2.20274708011188,0.0743054577980183));
#11930=CARTESIAN_POINT('Ctrl Pts',(99.1646375975492,-2.20080086652228,0.131999958697744));
#11931=CARTESIAN_POINT('Ctrl Pts',(99.1615001680201,-2.19658887303926,0.189545959249616));
#11932=CARTESIAN_POINT('Ctrl Pts',(99.1583627384911,-2.19014343654103,0.24675438674162));
#11933=CARTESIAN_POINT('Ctrl Pts',(99.1542897455551,-2.18177600801924,0.321022037662551));
#11934=CARTESIAN_POINT('Ctrl Pts',(99.1502167526192,-2.1696105373008,0.395006868667691));
#11935=CARTESIAN_POINT('Ctrl Pts',(99.1461437596832,-2.15367606013578,0.468289897390542));
#11936=CARTESIAN_POINT('Ctrl Pts',(99.1420767520201,-2.13776499872324,0.541465236526569));
#11937=CARTESIAN_POINT('Ctrl Pts',(99.1380097443571,-2.11809602776835,0.613940358226609));
#11938=CARTESIAN_POINT('Ctrl Pts',(99.133942736694,-2.09474986256318,0.685302132852038));
#11939=CARTESIAN_POINT('Ctrl Pts',(99.1298804888272,-2.07143102039191,0.75658038968468));
#11940=CARTESIAN_POINT('Ctrl Pts',(99.1258182409603,-2.04444368191489,0.826747436671027));
#11941=CARTESIAN_POINT('Ctrl Pts',(99.1217559930934,-2.01391907905545,0.895402670878566));
#11942=CARTESIAN_POINT('Ctrl Pts',(99.117696324253,-1.98341385555471,0.964014317478532));
#11943=CARTESIAN_POINT('Ctrl Pts',(99.1136366554126,-1.94937601755784,1.03111562075139));
#11944=CARTESIAN_POINT('Ctrl Pts',(99.1095769865722,-1.91198540020253,1.09632469160025));
#11945=CARTESIAN_POINT('Ctrl Pts',(99.105518583105,-1.87460643726626,1.16151343719398));
#11946=CARTESIAN_POINT('Ctrl Pts',(99.1014601796377,-1.83387700720655,1.22481070743143));
#11947=CARTESIAN_POINT('Ctrl Pts',(99.0974017761704,-1.79002274859216,1.28585946336392));
#11948=CARTESIAN_POINT('Ctrl Pts',(99.0933433261073,-1.74616798647374,1.34690892021569));
#11949=CARTESIAN_POINT('Ctrl Pts',(99.0892848760443,-1.69918860459373,1.40570942475502));
#11950=CARTESIAN_POINT('Ctrl Pts',(99.0852264259812,-1.64935245476583,1.46193449920232));
#11951=CARTESIAN_POINT('Ctrl Pts',(99.0811638259375,-1.59946534482858,1.51821706677362));
#11952=CARTESIAN_POINT('Ctrl Pts',(99.0771012258938,-1.54671595089979,1.57191858716061));
#11953=CARTESIAN_POINT('Ctrl Pts',(99.07303862585,-1.49141066508986,1.62274774011743));
#11954=CARTESIAN_POINT('Ctrl Pts',(99.0689739041421,-1.43607649648385,1.67360343824147));
#11955=CARTESIAN_POINT('Ctrl Pts',(99.064909182434,-1.37818414585655,1.72158347671752));
#11956=CARTESIAN_POINT('Ctrl Pts',(99.060844460726,-1.31807288491114,1.76643705522219));
#11957=CARTESIAN_POINT('Ctrl Pts',(99.0567724774148,-1.25785423552448,1.81137076440128));
#11958=CARTESIAN_POINT('Ctrl Pts',(99.0527004941035,-1.19540915528624,1.8531665912189));
#11959=CARTESIAN_POINT('Ctrl Pts',(99.0486285107923,-1.13110527439736,1.89161752429778));
#11960=CARTESIAN_POINT('Ctrl Pts',(99.0454896813522,-1.08153755787727,1.92125686992423));
#11961=CARTESIAN_POINT('Ctrl Pts',(99.0423508519121,-1.03086596171574,1.94890961628639));
#11962=CARTESIAN_POINT('Ctrl Pts',(99.039212022472,-0.97926716831074,1.97450039581375));
#11963=CARTESIAN_POINT('Ctrl Pts',(99.0346322578875,-0.90398103660152,2.01183907509093));
#11964=CARTESIAN_POINT('Ctrl Pts',(99.0300524933029,-0.826449303819452,
2.04492059732323));
#11965=CARTESIAN_POINT('Ctrl Pts',(99.0254727287184,-0.74716224320077,2.07349091686826));
#11966=CARTESIAN_POINT('Ctrl Pts',(99.0211239147306,-0.671873509051896,
2.10062047843846));
#11967=CARTESIAN_POINT('Ctrl Pts',(99.0167751007428,-0.595002578912433,
2.12368253475061));
#11968=CARTESIAN_POINT('Ctrl Pts',(99.012426286755,-0.516994574433637,2.14250615168456));
#11969=CARTESIAN_POINT('Ctrl Pts',(99.0080869948121,-0.439157374160702,
2.16128855293861));
#11970=CARTESIAN_POINT('Ctrl Pts',(99.0037477028693,-0.360188413294784,
2.17585089502794));
#11971=CARTESIAN_POINT('Ctrl Pts',(98.9994084109264,-0.28054952401915,2.18607135395271));
#11972=CARTESIAN_POINT('Ctrl Pts',(98.99508172104,-0.201141919892249,2.19626213089191));
#11973=CARTESIAN_POINT('Ctrl Pts',(98.9907550311536,-0.121068629902613,
2.20213609041139));
#11974=CARTESIAN_POINT('Ctrl Pts',(98.9864283412672,-0.0408017934233111,
2.20362229378209));
#11975=CARTESIAN_POINT('Ctrl Pts',(98.9857038433307,-0.0273612282512411,
2.20387115637764));
#11976=CARTESIAN_POINT('Ctrl Pts',(98.9849793453942,-0.0139152616418334,
2.2039971062624));
#11977=CARTESIAN_POINT('Ctrl Pts',(98.9842548474577,-0.000466138566033943,
2.20399995070663));
#11978=CARTESIAN_POINT('',(98.2342548473827,0.00202208611722839,2.20399907240628));
#11979=CARTESIAN_POINT('Ctrl Pts',(98.9842548474101,-0.000466137681637975,
2.20399995070682));
#11980=CARTESIAN_POINT('Ctrl Pts',(98.9800659211421,0.0772944494749427,
2.20401639677789));
#11981=CARTESIAN_POINT('Ctrl Pts',(98.975876994874,0.155004589942922,2.1999132369169));
#11982=CARTESIAN_POINT('Ctrl Pts',(98.971688068606,0.232216947609706,2.19173248578444));
#11983=CARTESIAN_POINT('Ctrl Pts',(98.9673858384265,0.311517778926223,2.18333045811424));
#11984=CARTESIAN_POINT('Ctrl Pts',(98.9630836082471,0.390293025390627,2.17062713283996));
#11985=CARTESIAN_POINT('Ctrl Pts',(98.9587813780677,0.468068877566995,2.15372410625251));
#11986=CARTESIAN_POINT('Ctrl Pts',(98.9545794155905,0.544032087074628,2.13721502131104));
#11987=CARTESIAN_POINT('Ctrl Pts',(98.9503774531134,0.619041586376206,2.11670007151106));
#11988=CARTESIAN_POINT('Ctrl Pts',(98.9461754906363,0.692672418946442,2.0923242865366));
#11989=CARTESIAN_POINT('Ctrl Pts',(98.9418231266057,0.768938732357677,2.06707601496865));
#11990=CARTESIAN_POINT('Ctrl Pts',(98.9374707625751,0.843725343475413,2.03768550765046));
#11991=CARTESIAN_POINT('Ctrl Pts',(98.9331183985445,0.916585256674168,2.00436709892364));
#11992=CARTESIAN_POINT('Ctrl Pts',(98.9287660345139,0.989445169872913,1.97104869019682));
#11993=CARTESIAN_POINT('Ctrl Pts',(98.9244136704833,1.06037797311012,1.93380268451775));
#11994=CARTESIAN_POINT('Ctrl Pts',(98.9200613064528,1.12896878897367,1.89289341314384));
#11995=CARTESIAN_POINT('Ctrl Pts',(98.9159882345174,1.19315811807277,1.85460929812984));
#11996=CARTESIAN_POINT('Ctrl Pts',(98.911915162582,1.2555216575691,1.81298260017475));
#11997=CARTESIAN_POINT('Ctrl Pts',(98.9078420906466,1.31568978311253,1.76821276847932));
#11998=CARTESIAN_POINT('Ctrl Pts',(98.9037750026509,1.37576951286062,1.72350871022863));
#11999=CARTESIAN_POINT('Ctrl Pts',(98.8997079146552,1.43365985248843,1.6756709689612));
#12000=CARTESIAN_POINT('Ctrl Pts',(98.8956408266595,1.4890178468179,1.62494364574831));
#12001=CARTESIAN_POINT('Ctrl Pts',(98.8915784968471,1.5443110765083,1.57427566964179));
#12002=CARTESIAN_POINT('Ctrl Pts',(98.8875161670347,1.59707749676501,1.52072514900194));
#12003=CARTESIAN_POINT('Ctrl Pts',(98.8834538372224,1.64700641957879,1.46457702216929));
#12004=CARTESIAN_POINT('Ctrl Pts',(98.8793940854881,1.69690365597848,1.40846452864689));
#12005=CARTESIAN_POINT('Ctrl Pts',(98.8753343337539,1.74396665188229,1.34975805613334));
#12006=CARTESIAN_POINT('Ctrl Pts',(98.8712745820197,1.78792183141841,1.28877908298413));
#12007=CARTESIAN_POINT('Ctrl Pts',(98.867216094829,1.83186331966421,1.22781910374723));
#12008=CARTESIAN_POINT('Ctrl Pts',(98.8631576076384,1.87269863451879,1.16458841634131));
#12009=CARTESIAN_POINT('Ctrl Pts',(98.8590991204477,1.91019574487544,1.09943995573191));
#12010=CARTESIAN_POINT('Ctrl Pts',(98.8550405859496,1.94769329231425,1.03429073572453));
#12011=CARTESIAN_POINT('Ctrl Pts',(98.8509820514515,1.98185232137401,0.967224112833762));
#12012=CARTESIAN_POINT('Ctrl Pts',(98.8469235169534,2.01248606470643,0.898618850994355));
#12013=CARTESIAN_POINT('Ctrl Pts',(98.8428608319543,2.04315113594403,0.829943429295143));
#12014=CARTESIAN_POINT('Ctrl Pts',(98.8387981469551,2.07028352703557,0.75972666338779));
#12015=CARTESIAN_POINT('Ctrl Pts',(98.8347354619559,2.09374440406664,0.688367903406034));
#12016=CARTESIAN_POINT('Ctrl Pts',(98.8306706548699,2.11721753555982,0.616971870170623));
#12017=CARTESIAN_POINT('Ctrl Pts',(98.8266058477839,2.13701520812239,0.544433116020145));
#12018=CARTESIAN_POINT('Ctrl Pts',(98.8225410406978,2.15304906800389,0.471164207859177));
#12019=CARTESIAN_POINT('Ctrl Pts',(98.818468972282,2.16911157060874,0.397764412869827));
#12020=CARTESIAN_POINT('Ctrl Pts',(98.8143969038661,2.18139675241525,0.323632330286333));
#12021=CARTESIAN_POINT('Ctrl Pts',(98.8103248354503,2.18986785055103,0.249188276455825));
#12022=CARTESIAN_POINT('Ctrl Pts',(98.8071867537781,2.19639598197921,0.19181902400911));
#12023=CARTESIAN_POINT('Ctrl Pts',(98.8040486721059,2.20066006838065,0.134264671864022));
#12024=CARTESIAN_POINT('Ctrl Pts',(98.8009105904337,2.20266440573115,0.0767171149422006));
#12025=CARTESIAN_POINT('Ctrl Pts',(98.796837534475,2.20526592444271,0.00202357789872107));
#12026=CARTESIAN_POINT('Ctrl Pts',(98.7927644785163,2.20406880647379,-0.0729464854661871));
#12027=CARTESIAN_POINT('Ctrl Pts',(98.7886914225577,2.19904041407215,-0.147774345802607));
#12028=CARTESIAN_POINT('Ctrl Pts',(98.7846243508788,2.19401940956488,-0.222492266364284));
#12029=CARTESIAN_POINT('Ctrl Pts',(98.7805572792,2.18517833832298,-0.297067926274521));
#12030=CARTESIAN_POINT('Ctrl Pts',(98.7764902075211,2.17253654210778,-0.371080817621158));
#12031=CARTESIAN_POINT('Ctrl Pts',(98.7724278944578,2.15990953723449,-0.445007111306859));
#12032=CARTESIAN_POINT('Ctrl Pts',(98.7683655813945,2.14349072250751,-0.5183714763544));
#12033=CARTESIAN_POINT('Ctrl Pts',(98.7643032683311,2.12335124622355,-0.5907583982991));
#12034=CARTESIAN_POINT('Ctrl Pts',(98.7602435336027,2.10322455238986,-0.663099376535162));
#12035=CARTESIAN_POINT('Ctrl Pts',(98.7561837988743,2.07938201077449,-0.734463683918276));
#12036=CARTESIAN_POINT('Ctrl Pts',(98.7521240641459,2.05194558955012,-0.804447199961441));
#12037=CARTESIAN_POINT('Ctrl Pts',(98.7480655941936,2.02451771591133,-0.874408913230569));
#12038=CARTESIAN_POINT('Ctrl Pts',(98.7440071242412,1.99349835982372,-0.942990245018632));
#12039=CARTESIAN_POINT('Ctrl Pts',(98.7399486542889,1.95905843849026,-1.00980494877977));
#12040=CARTESIAN_POINT('Ctrl Pts',(98.7358901372377,1.92461811747864,-1.07662042793112));
#12041=CARTESIAN_POINT('Ctrl Pts',(98.7318316201865,1.88675737275609,-1.14166881476953));
#12042=CARTESIAN_POINT('Ctrl Pts',(98.7277731031353,1.84569335560361,-1.20458791172778));
#12043=CARTESIAN_POINT('Ctrl Pts',(98.7237104357869,1.80458734580317,-1.26757135064941));
#12044=CARTESIAN_POINT('Ctrl Pts',(98.7196477684384,1.76027178369827,-1.32842075073339));
#12045=CARTESIAN_POINT('Ctrl Pts',(98.71558510109,1.71300709461038,-1.386803047954));
#12046=CARTESIAN_POINT('Ctrl Pts',(98.7115203117955,1.66571771900266,-1.4452158384618));
#12047=CARTESIAN_POINT('Ctrl Pts',(98.7074555225011,1.6154764683021,-1.50115860446677));
#12048=CARTESIAN_POINT('Ctrl Pts',(98.7033907332066,1.56258222777984,-1.55433354896129));
#12049=CARTESIAN_POINT('Ctrl Pts',(98.6993186826129,1.50959349751127,-1.60760348464892));
#12050=CARTESIAN_POINT('Ctrl Pts',(98.6952466320192,1.45394266522222,-1.65809540144811));
#12051=CARTESIAN_POINT('Ctrl Pts',(98.6911745814255,1.39596308267522,-1.70555066527146));
#12052=CARTESIAN_POINT('Ctrl Pts',(98.6880363457552,1.35127955286296,-1.74212334487086));
#12053=CARTESIAN_POINT('Ctrl Pts',(98.6848981100848,1.30521359901653,-1.7768932234169));
#12054=CARTESIAN_POINT('Ctrl Pts',(98.6817598744145,1.25792886057399,-1.8097599237841));
#12055=CARTESIAN_POINT('Ctrl Pts',(98.6776868063584,1.19655872208867,-1.85241711127264));
#12056=CARTESIAN_POINT('Ctrl Pts',(98.6736137383024,1.13289797794599,-1.89203136868507));
#12057=CARTESIAN_POINT('Ctrl Pts',(98.6695406702463,1.06728088726471,-1.92834838856454));
#12058=CARTESIAN_POINT('Ctrl Pts',(98.6654735862884,1.00176020035204,-1.96461205195495));
#12059=CARTESIAN_POINT('Ctrl Pts',(98.6614065023305,0.934289287714346,-1.99758786635259));
#12060=CARTESIAN_POINT('Ctrl Pts',(98.6573394183727,0.865232066629473,-2.02706424932119));
#12061=CARTESIAN_POINT('Ctrl Pts',(98.6532770928171,0.796255641035015,-2.05650614554416));
#12062=CARTESIAN_POINT('Ctrl Pts',(98.6492147672615,0.725697031260407,-2.0824565582041));
#12063=CARTESIAN_POINT('Ctrl Pts',(98.645152441706,0.653944027213801,-2.10475015364565));
#12064=CARTESIAN_POINT('Ctrl Pts',(98.6410926943609,0.582236562191627,-2.12702960015225));
#12065=CARTESIAN_POINT('Ctrl Pts',(98.6370329470157,0.509336661946798,-2.14565669360773));
#12066=CARTESIAN_POINT('Ctrl Pts',(98.6329731996706,0.435650074823647,-2.16051498775319));
#12067=CARTESIAN_POINT('Ctrl Pts',(98.6289147169952,0.361986442133028,-2.17536865332614));
#12068=CARTESIAN_POINT('Ctrl Pts',(98.6248562343198,0.287537076862959,-2.18645575627118));
#12069=CARTESIAN_POINT('Ctrl Pts',(98.6207977516444,0.212719225792712,-2.19371067622377));
#12070=CARTESIAN_POINT('Ctrl Pts',(98.6167392217818,0.13790050482908,-2.20096568052798));
#12071=CARTESIAN_POINT('Ctrl Pts',(98.6126806919192,0.062713764962516,-2.20438836907451));
#12072=CARTESIAN_POINT('Ctrl Pts',(98.6086221620565,-0.0124189096529951,
-2.20396501122024));
#12073=CARTESIAN_POINT('Ctrl Pts',(98.6045594818485,-0.0876284166600681,
-2.20354122043054));
#12074=CARTESIAN_POINT('Ctrl Pts',(98.6004968016404,-0.162783269495413,
-2.19926353185));
#12075=CARTESIAN_POINT('Ctrl Pts',(98.5964341214323,-0.237462423946303,
-2.19117037156255));
#12076=CARTESIAN_POINT('Ctrl Pts',(98.5923693192312,-0.312180584333164,
-2.18307298410763));
#12077=CARTESIAN_POINT('Ctrl Pts',(98.58830451703,-0.386422079680152,-2.17115623207429));
#12078=CARTESIAN_POINT('Ctrl Pts',(98.5842397148289,-0.459774669191026,
-2.15550997528898));
#12079=CARTESIAN_POINT('Ctrl Pts',(98.5801676513979,-0.533258293373165,
-2.13983576854133));
#12080=CARTESIAN_POINT('Ctrl Pts',(98.5760955879668,-0.605849378058541,
-2.1204188732418));
#12081=CARTESIAN_POINT('Ctrl Pts',(98.5720235245358,-0.677149924069375,
-2.09739933735396));
#12082=CARTESIAN_POINT('Ctrl Pts',(98.568885402489,-0.732097451084112,-2.07965940910893));
#12083=CARTESIAN_POINT('Ctrl Pts',(98.5657472804422,-0.786278811957624,
-2.05978092427929));
#12084=CARTESIAN_POINT('Ctrl Pts',(98.5626091583954,-0.839520996472622,
-2.03784702479887));
#12085=CARTESIAN_POINT('Ctrl Pts',(98.5585360928936,-0.908625671738396,
-2.00937833939999));
#12086=CARTESIAN_POINT('Ctrl Pts',(98.5544630273918,-0.976413882151996,
-1.97733569537347));
#12087=CARTESIAN_POINT('Ctrl Pts',(98.5503899618901,-1.04249077563177,-1.94186224607274));
#12088=CARTESIAN_POINT('Ctrl Pts',(98.5463228804995,-1.10847058953349,-1.90644091404492));
#12089=CARTESIAN_POINT('Ctrl Pts',(98.542255799109,-1.17274366113594,-1.86759900817242));
#12090=CARTESIAN_POINT('Ctrl Pts',(98.5381887177184,-1.23493497904427,-1.82552775863117));
#12091=CARTESIAN_POINT('Ctrl Pts',(98.5341263947373,-1.29705353427032,-1.78350573166738));
#12092=CARTESIAN_POINT('Ctrl Pts',(98.5300640717561,-1.35709478132595,-1.73826213378279));
#12093=CARTESIAN_POINT('Ctrl Pts',(98.5260017487749,-1.41470964593181,-1.69003331851993));
#12094=CARTESIAN_POINT('Ctrl Pts',(98.5219420040072,-1.47228794441086,-1.64183511238871));
#12095=CARTESIAN_POINT('Ctrl Pts',(98.5178822592395,-1.52744255109358,-1.59065575422982));
#12096=CARTESIAN_POINT('Ctrl Pts',(98.5138225144717,-1.57985575099939,-1.53677317976147));
#12097=CARTESIAN_POINT('Ctrl Pts',(98.509764034373,-1.63225262343827,-1.48290739049138));
#12098=CARTESIAN_POINT('Ctrl Pts',(98.5057055542742,-1.68190945195677,-1.42634039887376));
#12099=CARTESIAN_POINT('Ctrl Pts',(98.5016470741755,-1.72854501034008,-1.36738734352355));
#12100=CARTESIAN_POINT('Ctrl Pts',(98.497588546885,-1.77518111099854,-1.30843360267119));
#12101=CARTESIAN_POINT('Ctrl Pts',(98.4935300195945,-1.81879557695176,-1.24709411857095));
#12102=CARTESIAN_POINT('Ctrl Pts',(98.489471492304,-1.85914817399835,-1.1837162105499));
#12103=CARTESIAN_POINT('Ctrl Pts',(98.4854088146429,-1.89954203680996,-1.12027349039651));
#12104=CARTESIAN_POINT('Ctrl Pts',(98.4813461369818,-1.93666711254185,-1.05478858723801));
#12105=CARTESIAN_POINT('Ctrl Pts',(98.4772834593207,-1.97032756787706,-0.987636205929935));
#12106=CARTESIAN_POINT('Ctrl Pts',(98.4732186596566,-2.00400560461829,-0.920448749835463));
#12107=CARTESIAN_POINT('Ctrl Pts',(98.4691538599926,-2.03421522525858,-0.85159251881448));
#12108=CARTESIAN_POINT('Ctrl Pts',(98.4650890603285,-2.06080859611859,-0.781462686354086));
#12109=CARTESIAN_POINT('Ctrl Pts',(98.4610169993891,-2.08744947283495,-0.711207575388574));
#12110=CARTESIAN_POINT('Ctrl Pts',(98.4569449384496,-2.11046104999968,-0.639674773772419));
#12111=CARTESIAN_POINT('Ctrl Pts',(98.4528728775102,-2.12974539317599,-0.567274677952076));
#12112=CARTESIAN_POINT('Ctrl Pts',(98.4497347324655,-2.14460692567234,-0.511479343522763));
#12113=CARTESIAN_POINT('Ctrl Pts',(98.4465965874209,-2.15725585695442,-0.455169245346742));
#12114=CARTESIAN_POINT('Ctrl Pts',(98.4434584423762,-2.16766832644021,-0.398534849853682));
#12115=CARTESIAN_POINT('Ctrl Pts',(98.4393853785347,-2.18118288754535,-0.325027887880069));
#12116=CARTESIAN_POINT('Ctrl Pts',(98.4353123146932,-2.19098027329576,-0.25069096209894));
#12117=CARTESIAN_POINT('Ctrl Pts',(98.4312392508518,-2.19696686395659,-0.175933506407276));
#12118=CARTESIAN_POINT('Ctrl Pts',(98.4271721711602,-2.20294465911178,-0.101285884452472));
#12119=CARTESIAN_POINT('Ctrl Pts',(98.4231050914687,-2.2051227373313,-0.0262194312439857));
#12120=CARTESIAN_POINT('Ctrl Pts',(98.4190380117771,-2.20345863725056,0.0488470462354287));
#12121=CARTESIAN_POINT('Ctrl Pts',(98.4149756905449,-2.20179648415711,0.123825696377855));
#12122=CARTESIAN_POINT('Ctrl Pts',(98.4109133693126,-2.19630109447879,0.198803895789822));
#12123=CARTESIAN_POINT('Ctrl Pts',(98.4068510480804,-2.1869819860372,0.273360188668321));
#12124=CARTESIAN_POINT('Ctrl Pts',(98.4027913050913,-2.17766879217654,0.347869162725441));
#12125=CARTESIAN_POINT('Ctrl Pts',(98.3987315621023,-2.16453675436123,0.421956289040943));
#12126=CARTESIAN_POINT('Ctrl Pts',(98.3946718191132,-2.14764733110511,0.495203938995964));
#12127=CARTESIAN_POINT('Ctrl Pts',(98.3906133408203,-2.13076316926325,0.568428770751416));
#12128=CARTESIAN_POINT('Ctrl Pts',(98.3865548625275,-2.11012405317688,0.640814180423116));
#12129=CARTESIAN_POINT('Ctrl Pts',(98.3824963842346,-2.08584248054946,0.711953050653816));
#12130=CARTESIAN_POINT('Ctrl Pts',(98.3784378587748,-2.0615606257254,0.78309274764936));
#12131=CARTESIAN_POINT('Ctrl Pts',(98.3743793333149,-2.03363638623842,0.852985425154341));
#12132=CARTESIAN_POINT('Ctrl Pts',(98.370320807855,-2.00223151782014,0.921240983156772));
#12133=CARTESIAN_POINT('Ctrl Pts',(98.3662581320504,-1.97079453403554,0.98956634091825));
#12134=CARTESIAN_POINT('Ctrl Pts',(98.3621954562458,-1.93587001346819,1.05625080126569));
#12135=CARTESIAN_POINT('Ctrl Pts',(98.3581327804411,-1.89766678655087,1.12092674480614));
#12136=CARTESIAN_POINT('Ctrl Pts',(98.3540679826508,-1.85944360561686,1.18563646938975));
#12137=CARTESIAN_POINT('Ctrl Pts',(98.3500031848605,-1.8179385718371,1.24833518953764));
#12138=CARTESIAN_POINT('Ctrl Pts',(98.3459383870701,-1.77340372661367,1.30868453892936));
#12139=CARTESIAN_POINT('Ctrl Pts',(98.3418663280117,-1.728789325292,1.36914169511248));
#12140=CARTESIAN_POINT('Ctrl Pts',(98.3377942689532,-1.68113460494581,1.42724072791491));
#12141=CARTESIAN_POINT('Ctrl Pts',(98.3337222098947,-1.63073143823414,1.48267696291364));
#12142=CARTESIAN_POINT('Ctrl Pts',(98.3305840487155,-1.59188788051238,1.52539929038897));
#12143=CARTESIAN_POINT('Ctrl Pts',(98.3274458875363,-1.55141281655021,1.56654083295959));
#12144=CARTESIAN_POINT('Ctrl Pts',(98.3243077263571,-1.50945340650252,1.60597833534514));
#12145=CARTESIAN_POINT('Ctrl Pts',(98.3202847758764,-1.45566374460082,1.65653504996899));
#12146=CARTESIAN_POINT('Ctrl Pts',(98.3162618253957,-1.39921494262276,1.70449547284695));
#12147=CARTESIAN_POINT('Ctrl Pts',(98.3122388749149,-1.34039097563458,1.74956224022965));
#12148=CARTESIAN_POINT('Ctrl Pts',(98.3082213064714,-1.28164570530911,1.79456871578958));
#12149=CARTESIAN_POINT('Ctrl Pts',(98.3042037380278,-1.22053195433016,1.83668891555991));
#12150=CARTESIAN_POINT('Ctrl Pts',(98.3001861695843,-1.15736980930053,1.87566284937343));
#12151=CARTESIAN_POINT('Ctrl Pts',(98.2961726017163,-1.09427055926356,1.91459797409837));
#12152=CARTESIAN_POINT('Ctrl Pts',(98.2921590338484,-1.02912737514308,1.95039279055704));
#12153=CARTESIAN_POINT('Ctrl Pts',(98.2881454659804,-0.96229122060861,1.98282919252758));
#12154=CARTESIAN_POINT('Ctrl Pts',(98.2841345225613,-0.895498769848787,
2.0152443845226));
#12155=CARTESIAN_POINT('Ctrl Pts',(98.2801235791422,-0.827015985307934,
2.04430530678105));
#12156=CARTESIAN_POINT('Ctrl Pts',(98.276112635723,-0.757218903963501,2.06983949413483));
#12157=CARTESIAN_POINT('Ctrl Pts',(98.2721017199381,-0.687422303500887,
2.09537350556539));
#12158=CARTESIAN_POINT('Ctrl Pts',(98.2680908041532,-0.616311878717547,
2.11738064673258));
#12159=CARTESIAN_POINT('Ctrl Pts',(98.2640798883684,-0.544282841101875,
2.13573691939857));
#12160=CARTESIAN_POINT('Ctrl Pts',(98.2600690287855,-0.47225481277564,2.15409293485173));
#12161=CARTESIAN_POINT('Ctrl Pts',(98.2560581692025,-0.399308674593535,
2.16879807161835));
#12162=CARTESIAN_POINT('Ctrl Pts',(98.2520473096196,-0.325851804889479,
2.17977902578456));
#12163=CARTESIAN_POINT('Ctrl Pts',(98.2480331976153,-0.252335368727682,
2.19076888444867));
#12164=CARTESIAN_POINT('Ctrl Pts',(98.2440190856109,-0.178307861136477,
2.198028472553));
#12165=CARTESIAN_POINT('Ctrl Pts',(98.2400049736066,-0.104182596936714,
2.20153627871437));
#12166=CARTESIAN_POINT('Ctrl Pts',(98.2380882648744,-0.06878833264788,2.20321123015893));
#12167=CARTESIAN_POINT('Ctrl Pts',(98.2361715561422,-0.0333718065489038,
2.20403154496129));
#12168=CARTESIAN_POINT('Ctrl Pts',(98.23425484741,0.00202208561227388,2.20399907240674));
#12169=CARTESIAN_POINT('',(97.484254847371,-0.00067182755121702,2.20399989760611));
#12170=CARTESIAN_POINT('Ctrl Pts',(98.2342548473827,0.00202208611721571,
2.20399907240628));
#12171=CARTESIAN_POINT('Ctrl Pts',(98.2289277772449,0.100391620738078,2.20390882206416));
#12172=CARTESIAN_POINT('Ctrl Pts',(98.2236007071072,0.198467672311368,2.19722915975478));
#12173=CARTESIAN_POINT('Ctrl Pts',(98.2182736369695,0.295508944404814,2.18409946288551));
#12174=CARTESIAN_POINT('Ctrl Pts',(98.2139014280923,0.375155861064196,2.17332322459276));
#12175=CARTESIAN_POINT('Ctrl Pts',(98.2095292192152,0.454106399944636,2.15820294185027));
#12176=CARTESIAN_POINT('Ctrl Pts',(98.205157010338,0.531962637762755,2.138838879398));
#12177=CARTESIAN_POINT('Ctrl Pts',(98.2010839453725,0.604491998439037,2.12079969449621));
#12178=CARTESIAN_POINT('Ctrl Pts',(98.197010880407,0.676242606939927,2.0990322666232));
#12179=CARTESIAN_POINT('Ctrl Pts',(98.1929378154415,0.746802901210407,2.07362036707391));
#12180=CARTESIAN_POINT('Ctrl Pts',(98.188870734605,0.817259528608114,2.04824580257522));
#12181=CARTESIAN_POINT('Ctrl Pts',(98.1848036537686,0.88652886837879,2.01923755759146));
#12182=CARTESIAN_POINT('Ctrl Pts',(98.1807365729321,0.954211942849043,1.98672986792977));
#12183=CARTESIAN_POINT('Ctrl Pts',(98.1766742505292,1.02181582897173,1.95426021185696));
#12184=CARTESIAN_POINT('Ctrl Pts',(98.1726119281263,1.08783670883466,1.91829945123413));
#12185=CARTESIAN_POINT('Ctrl Pts',(98.1685496057233,1.15189465244276,1.87903025778559));
#12186=CARTESIAN_POINT('Ctrl Pts',(98.1644898615484,1.21591194049374,1.839785987256));
#12187=CARTESIAN_POINT('Ctrl Pts',(98.1604301173734,1.27796835844299,1.79723769955032));
#12188=CARTESIAN_POINT('Ctrl Pts',(98.1563703731984,1.33770890638433,1.75161379355726));
#12189=CARTESIAN_POINT('Ctrl Pts',(98.1523118937061,1.39743084408001,1.70600410022423));
#12190=CARTESIAN_POINT('Ctrl Pts',(98.1482534142138,1.45483796493468,1.65732098049386));
#12191=CARTESIAN_POINT('Ctrl Pts',(98.1441949347215,1.50960591474826,1.60583497974015));
#12192=CARTESIAN_POINT('Ctrl Pts',(98.1401364080503,1.56437450122625,1.55434838047393));
#12193=CARTESIAN_POINT('Ctrl Pts',(98.1360778813792,1.61650350909749,1.50005916382788));
#12194=CARTESIAN_POINT('Ctrl Pts',(98.132019354708,1.66570442019289,1.44327571328207));
#12195=CARTESIAN_POINT('Ctrl Pts',(98.127956677682,1.71495564541824,1.38643419450447));
#12196=CARTESIAN_POINT('Ctrl Pts',(98.123894000656,1.76127248096927,1.32709370993731));
#12197=CARTESIAN_POINT('Ctrl Pts',(98.11983132363,1.80440631920992,1.26559623703428));
#12198=CARTESIAN_POINT('Ctrl Pts',(98.1157665246109,1.84756268685913,1.20406664313878));
#12199=CARTESIAN_POINT('Ctrl Pts',(98.1117017255917,1.8875324924024,1.14037822213482));
#12200=CARTESIAN_POINT('Ctrl Pts',(98.1076369265725,1.92411161185864,1.07490023030547));
#12201=CARTESIAN_POINT('Ctrl Pts',(98.1035648662868,1.96075607544003,1.00930527004832));
#12202=CARTESIAN_POINT('Ctrl Pts',(98.0994928060011,1.99399754292445,0.941914782343538));
#12203=CARTESIAN_POINT('Ctrl Pts',(98.0954207457154,2.02367902148731,0.873120391465089));
#12204=CARTESIAN_POINT('Ctrl Pts',(98.0922825952499,2.04655317835997,0.820103703446003));
#12205=CARTESIAN_POINT('Ctrl Pts',(98.0891444447844,2.0673139948512,0.76625369991621));
#12206=CARTESIAN_POINT('Ctrl Pts',(98.0860062943188,2.08590996800986,0.711755298791019));
#12207=CARTESIAN_POINT('Ctrl Pts',(98.0819332295131,2.11004603306881,0.641020793855812));
#12208=CARTESIAN_POINT('Ctrl Pts',(98.0778601647074,2.13062658797387,0.568920787013463));
#12209=CARTESIAN_POINT('Ctrl Pts',(98.0737870999016,2.14749904921425,0.495846582749047));
#12210=CARTESIAN_POINT('Ctrl Pts',(98.0697200192292,2.16434672149054,0.42287973886312));
#12211=CARTESIAN_POINT('Ctrl Pts',(98.0656529385568,2.17749700991872,0.348942000603794));
#12212=CARTESIAN_POINT('Ctrl Pts',(98.0615858578843,2.18684656459241,0.274441438070829));
#12213=CARTESIAN_POINT('Ctrl Pts',(98.057523535651,2.19618518039122,0.200028040366577));
#12214=CARTESIAN_POINT('Ctrl Pts',(98.0534612134177,2.20173183808983,0.125053598038256));
#12215=CARTESIAN_POINT('Ctrl Pts',(98.0493988911844,2.20343421831169,0.0499364153015492));
#12216=CARTESIAN_POINT('Ctrl Pts',(98.0453391471823,2.20513551808505,-0.0251330928639777));
#12217=CARTESIAN_POINT('Ctrl Pts',(98.0412794031803,2.20299737119982,-0.100344685537534));
#12218=CARTESIAN_POINT('Ctrl Pts',(98.0372196591782,2.19701939932981,-0.175276236177271));
#12219=CARTESIAN_POINT('Ctrl Pts',(98.0331611798619,2.19104328970924,-0.250184444245087));
#12220=CARTESIAN_POINT('Ctrl Pts',(98.0291027005457,2.18122976800794,-0.324812307849021));
#12221=CARTESIAN_POINT('Ctrl Pts',(98.0250442212294,2.16763048424939,-0.39874062215023));
#12222=CARTESIAN_POINT('Ctrl Pts',(98.0209856947371,2.15403104241195,-0.472669795798605));
#12223=CARTESIAN_POINT('Ctrl Pts',(98.0169271682449,2.13664583928596,-0.545898934741146));
#12224=CARTESIAN_POINT('Ctrl Pts',(98.0128686417526,2.11557774430185,-0.618018452649033));
#12225=CARTESIAN_POINT('Ctrl Pts',(98.0088059649087,2.09448810455213,-0.690211721795935));
#12226=CARTESIAN_POINT('Ctrl Pts',(98.0047432880648,2.06970818620269,-0.761292644600529));
#12227=CARTESIAN_POINT('Ctrl Pts',(98.000680611221,2.04139071857128,-0.830866977398324));
#12228=CARTESIAN_POINT('Ctrl Pts',(97.996615812386,2.01305846034317,-0.900477649812031));
#12229=CARTESIAN_POINT('Ctrl Pts',(97.992551013551,1.98118517587959,-0.968579732315303));
#12230=CARTESIAN_POINT('Ctrl Pts',(97.988486214716,1.94597062435514,-1.03480158926573));
#12231=CARTESIAN_POINT('Ctrl Pts',(97.9844141546157,1.91069316634791,-1.1011417434519));
#12232=CARTESIAN_POINT('Ctrl Pts',(97.9803420945155,1.8720627649595,-1.16559455301516));
#12233=CARTESIAN_POINT('Ctrl Pts',(97.9762700344153,1.83032351616074,-1.22781587633855));
#12234=CARTESIAN_POINT('Ctrl Pts',(97.9731318823768,1.79815697011727,-1.27576702829188));
#12235=CARTESIAN_POINT('Ctrl Pts',(97.9699937303382,1.76414497408377,-1.32239343605571));
#12236=CARTESIAN_POINT('Ctrl Pts',(97.9668555782997,1.72841504534132,-1.36755161914926));
#12237=CARTESIAN_POINT('Ctrl Pts',(97.9627825133003,1.68204051650868,-1.42616325196266));
#12238=CARTESIAN_POINT('Ctrl Pts',(97.9587094483009,1.63259184260637,-1.48252635568421));
#12239=CARTESIAN_POINT('Ctrl Pts',(97.9546363833014,1.58031523996454,-1.53630066794746));
#12240=CARTESIAN_POINT('Ctrl Pts',(97.9505693024321,1.52811544188933,-1.58999597521537));
#12241=CARTESIAN_POINT('Ctrl Pts',(97.9465022215628,1.47309629406208,-1.64110970290096));
#12242=CARTESIAN_POINT('Ctrl Pts',(97.9424351406935,1.41554477998905,-1.6893338852476));
#12243=CARTESIAN_POINT('Ctrl Pts',(97.9383728182595,1.35806060048928,-1.73750164588594));
#12244=CARTESIAN_POINT('Ctrl Pts',(97.9343104958254,1.29805030535379,-1.78278627281644));
#12245=CARTESIAN_POINT('Ctrl Pts',(97.9302481733914,1.23583712918931,-1.82491714609654));
#12246=CARTESIAN_POINT('Ctrl Pts',(97.9261884291864,1.17366343778255,-1.86702128022864));
#12247=CARTESIAN_POINT('Ctrl Pts',(97.9221286849814,1.10929003406122,-1.90597536560161));
#12248=CARTESIAN_POINT('Ctrl Pts',(97.9180689407764,1.0430715079989,-1.94155036741283));
#12249=CARTESIAN_POINT('Ctrl Pts',(97.9140104612552,0.976873610206266,-1.97711428696694));
#12250=CARTESIAN_POINT('Ctrl Pts',(97.909951981734,0.908832151622473,-2.00930098712529));
#12251=CARTESIAN_POINT('Ctrl Pts',(97.9058935022128,0.839327456571355,-2.03792674565242));
#12252=CARTESIAN_POINT('Ctrl Pts',(97.901834975514,0.769821953564913,-2.06655283693885));
#12253=CARTESIAN_POINT('Ctrl Pts',(97.8977764488151,0.698853622484897,-2.09161772423588));
#12254=CARTESIAN_POINT('Ctrl Pts',(97.8937179221163,0.626822455076543,-2.11298594643027));
#12255=CARTESIAN_POINT('Ctrl Pts',(97.8896552450646,0.554717626761799,-2.13437602031291));
#12256=CARTESIAN_POINT('Ctrl Pts',(97.885592568013,0.481548250435302,-2.15206174394929));
#12257=CARTESIAN_POINT('Ctrl Pts',(97.8815298909614,0.40772843753002,-2.16595787614379));
#12258=CARTESIAN_POINT('Ctrl Pts',(97.8774650919177,0.333870067521403,-2.17986126647922));
#12259=CARTESIAN_POINT('Ctrl Pts',(97.8734002928739,0.259361057956396,-2.18997105942271));
#12260=CARTESIAN_POINT('Ctrl Pts',(97.8693354938302,0.184622000096624,-2.19625379159156));
#12261=CARTESIAN_POINT('Ctrl Pts',(97.8652634335221,0.109749430086021,-2.20254774709008));
#12262=CARTESIAN_POINT('Ctrl Pts',(97.8611913732139,0.0346464688482193,
-2.20500097067697));
#12263=CARTESIAN_POINT('Ctrl Pts',(97.8571193129057,-0.0402653783392436,
-2.20363216061738));
#12264=CARTESIAN_POINT('Ctrl Pts',(97.8539811626974,-0.0979965048629268,
-2.20257728145334));
#12265=CARTESIAN_POINT('Ctrl Pts',(97.850843012489,-0.155614094320053,-2.19925354133635));
#12266=CARTESIAN_POINT('Ctrl Pts',(97.8477048622806,-0.21292846106124,-2.19369037707469));
#12267=CARTESIAN_POINT('Ctrl Pts',(97.8436317973462,-0.287317869440097,
-2.18646984020636));
#12268=CARTESIAN_POINT('Ctrl Pts',(97.8395587324119,-0.36148303709724,-2.17544720311697));
#12269=CARTESIAN_POINT('Ctrl Pts',(97.8354856674776,-0.435004570433692,
-2.16064504805898));
#12270=CARTESIAN_POINT('Ctrl Pts',(97.8314185866741,-0.508418086226198,
-2.14586464026825));
#12271=CARTESIAN_POINT('Ctrl Pts',(97.8273515058705,-0.581189380966512,
-2.12731583264171));
#12272=CARTESIAN_POINT('Ctrl Pts',(97.823284425067,-0.65290411767467,-2.10507297097356));
#12273=CARTESIAN_POINT('Ctrl Pts',(97.8192221026994,-0.724534948997614,
-2.08285613318785));
#12274=CARTESIAN_POINT('Ctrl Pts',(97.8151597803318,-0.795111224518574,
-2.05695396891655));
#12275=CARTESIAN_POINT('Ctrl Pts',(97.8110974579642,-0.864230354606361,
-2.02749152752286));
#12276=CARTESIAN_POINT('Ctrl Pts',(97.807037713826,-0.933305616936154,-1.99804778502262));
#12277=CARTESIAN_POINT('Ctrl Pts',(97.8029779696879,-1.00092513089808,-1.96504843607286));
#12278=CARTESIAN_POINT('Ctrl Pts',(97.7989182255497,-1.06670426994776,-1.92866741572393));
#12279=CARTESIAN_POINT('Ctrl Pts',(97.7948597460956,-1.13246291759979,-1.89229772872422));
#12280=CARTESIAN_POINT('Ctrl Pts',(97.7908012666416,-1.19638191108074,-1.85254869284278));
#12281=CARTESIAN_POINT('Ctrl Pts',(97.7867427871875,-1.25810076539643,-1.80964042398177));
#12282=CARTESIAN_POINT('Ctrl Pts',(97.7826842605559,-1.31982033715831,-1.76673165633681));
#12283=CARTESIAN_POINT('Ctrl Pts',(97.7786257339244,-1.37933932796847,-1.72066385681412));
#12284=CARTESIAN_POINT('Ctrl Pts',(97.7745672072928,-1.43632715981332,-1.67169982053675));
#12285=CARTESIAN_POINT('Ctrl Pts',(97.7705045303083,-1.49337326886991,-1.62268571238584));
#12286=CARTESIAN_POINT('Ctrl Pts',(97.7664418533238,-1.54788268706758,-1.57076976485147));
#12287=CARTESIAN_POINT('Ctrl Pts',(97.7623791763393,-1.59955939560565,-1.51625385075511));
#12288=CARTESIAN_POINT('Ctrl Pts',(97.7583143773627,-1.6512630955995,-1.46170946224685));
#12289=CARTESIAN_POINT('Ctrl Pts',(97.7542495783862,-1.7001308289334,-1.40456276606914));
#12290=CARTESIAN_POINT('Ctrl Pts',(97.7501847794096,-1.74590658485429,-1.34514913558401));
#12291=CARTESIAN_POINT('Ctrl Pts',(97.7461127191678,-1.7917641135529,-1.28562936992972));
#12292=CARTESIAN_POINT('Ctrl Pts',(97.742040658926,-1.83451836013391,-1.2238349744318));
#12293=CARTESIAN_POINT('Ctrl Pts',(97.7379685986842,-1.87395666017458,-1.16013035292907));
#12294=CARTESIAN_POINT('Ctrl Pts',(97.7348304478766,-1.90434995638714,-1.11103611130495));
#12295=CARTESIAN_POINT('Ctrl Pts',(97.731692297069,-1.93277477065016,-1.06080798103647));
#12296=CARTESIAN_POINT('Ctrl Pts',(97.7285541462614,-1.95915306880777,-1.00962134138553));
#12297=CARTESIAN_POINT('Ctrl Pts',(97.7244810813405,-1.99338995781841,-0.943185239629218));
#12298=CARTESIAN_POINT('Ctrl Pts',(97.7204080164196,-2.02430970542024,-0.874877554951377));
#12299=CARTESIAN_POINT('Ctrl Pts',(97.7163349514987,-2.05170405580196,-0.805063020766566));
#12300=CARTESIAN_POINT('Ctrl Pts',(97.712267870709,-2.07905815851011,-0.7353510578252));
#12301=CARTESIAN_POINT('Ctrl Pts',(97.7082007899193,-2.10289697446296,-0.664137081565813));
#12302=CARTESIAN_POINT('Ctrl Pts',(97.7041337091296,-2.12305849458596,-0.591809621894051));
#12303=CARTESIAN_POINT('Ctrl Pts',(97.7000713867765,-2.14319642596823,-0.519566784496978));
#12304=CARTESIAN_POINT('Ctrl Pts',(97.6960090644233,-2.15966548183138,-0.446213509594031));
#12305=CARTESIAN_POINT('Ctrl Pts',(97.6919467420702,-2.17235263411151,-0.372155925747258));
#12306=CARTESIAN_POINT('Ctrl Pts',(97.6878869979468,-2.18503173425028,-0.298145343947892));
#12307=CARTESIAN_POINT('Ctrl Pts',(97.6838272538235,-2.19393361343885,-0.223431809645988));
#12308=CARTESIAN_POINT('Ctrl Pts',(97.6797675097001,-2.19899606451928,-0.148432840802502));
#12309=CARTESIAN_POINT('Ctrl Pts',(97.6757090302612,-2.20405693855375,-0.0734572355075946));
#12310=CARTESIAN_POINT('Ctrl Pts',(97.6716505508223,-2.20528072705553,0.00180315171998274));
#12311=CARTESIAN_POINT('Ctrl Pts',(97.6675920713834,-2.20265711799268,0.0769260720184203));
#12312=CARTESIAN_POINT('Ctrl Pts',(97.6635335447673,-2.20003347843209,0.152049865571672));
#12313=CARTESIAN_POINT('Ctrl Pts',(97.6594750181512,-2.19356237096343,0.227035711915739));
#12314=CARTESIAN_POINT('Ctrl Pts',(97.6554164915351,-2.18328555940878,0.301463374354331));
#12315=CARTESIAN_POINT('Ctrl Pts',(97.6513538145665,-2.1729982385252,0.375967148413867));
#12316=CARTESIAN_POINT('Ctrl Pts',(97.6472911375978,-2.1588975072858,0.449911124662818));
#12317=CARTESIAN_POINT('Ctrl Pts',(97.6432284606292,-2.14107669898293,0.522882940123679));
#12318=CARTESIAN_POINT('Ctrl Pts',(97.6391636616687,-2.12324658262773,0.595892869763449));
#12319=CARTESIAN_POINT('Ctrl Pts',(97.6350988627082,-2.10169265681259,0.667929169585409));
#12320=CARTESIAN_POINT('Ctrl Pts',(97.6310340637477,-2.07655808902178,0.738594951863493));
#12321=CARTESIAN_POINT('Ctrl Pts',(97.6269620035222,-2.05137862140724,0.809386969897618));
#12322=CARTESIAN_POINT('Ctrl Pts',(97.6228899432968,-2.02260591864279,0.87880313844883));
#12323=CARTESIAN_POINT('Ctrl Pts',(97.6188178830713,-1.99043103409202,0.946467272822127));
#12324=CARTESIAN_POINT('Ctrl Pts',(97.6156797321283,-1.96563531921958,0.998612932594857));
#12325=CARTESIAN_POINT('Ctrl Pts',(97.6125415811853,-1.93882001339638,1.04971845874858));
#12326=CARTESIAN_POINT('Ctrl Pts',(97.6094034302423,-1.91009024138284,1.09962323992086));
#12327=CARTESIAN_POINT('Ctrl Pts',(97.6053303652977,-1.87280133164568,1.1643955910453));
#12328=CARTESIAN_POINT('Ctrl Pts',(97.6012573003531,-1.83214207195564,1.22739396603369));
#12329=CARTESIAN_POINT('Ctrl Pts',(97.5971842354084,-1.78830618136827,1.28824570702954));
#12330=CARTESIAN_POINT('Ctrl Pts',(97.5931171545946,-1.74453469429696,1.3490080448896));
#12331=CARTESIAN_POINT('Ctrl Pts',(97.5890500737809,-1.69759611917393,1.40762962619744));
#12332=CARTESIAN_POINT('Ctrl Pts',(97.584982992967,-1.64772923329867,1.46376376978424));
#12333=CARTESIAN_POINT('Ctrl Pts',(97.5809206705893,-1.59792069108524,1.51983223709243));
#12334=CARTESIAN_POINT('Ctrl Pts',(97.5768583482115,-1.54519096048288,1.57341869356677));
#12335=CARTESIAN_POINT('Ctrl Pts',(97.5727960258338,-1.4898201492766,1.6242080909814));
#12336=CARTESIAN_POINT('Ctrl Pts',(97.5687362816855,-1.43448448019958,1.6749652539474));
#12337=CARTESIAN_POINT('Ctrl Pts',(97.5646765375372,-1.37651140774591,1.72292855863136));
#12338=CARTESIAN_POINT('Ctrl Pts',(97.560616793389,-1.31621814823417,1.76781950047481));
#12339=CARTESIAN_POINT('Ctrl Pts',(97.5565583139249,-1.25594367117006,1.8126964579729));
#12340=CARTESIAN_POINT('Ctrl Pts',(97.5524998344608,-1.19335082481708,1.85450266795433));
#12341=CARTESIAN_POINT('Ctrl Pts',(97.5484413549967,-1.1287889196328,1.89300068011457));
#12342=CARTESIAN_POINT('Ctrl Pts',(97.5443828283553,-1.06422626395504,1.93149913979115));
#12343=CARTESIAN_POINT('Ctrl Pts',(97.5403243017138,-0.997694915004834,
1.96668908229734));
#12344=CARTESIAN_POINT('Ctrl Pts',(97.5362657750723,-0.929570707792732,
1.99837791701513));
#12345=CARTESIAN_POINT('Ctrl Pts',(97.5322030980781,-0.861376835031043,
2.03009915754249));
#12346=CARTESIAN_POINT('Ctrl Pts',(97.5281404210839,-0.791587285070047,
2.05831193875905));
#12347=CARTESIAN_POINT('Ctrl Pts',(97.5240777440897,-0.720599216502606,
2.08287128003049));
#12348=CARTESIAN_POINT('Ctrl Pts',(97.5200129451035,-0.649574069892286,
2.10744344898306));
#12349=CARTESIAN_POINT('Ctrl Pts',(97.5159481461174,-0.577349617097396,
2.12835824498218));
#12350=CARTESIAN_POINT('Ctrl Pts',(97.5118833471312,-0.504337011039581,
2.14552095755219));
#12351=CARTESIAN_POINT('Ctrl Pts',(97.5078112868801,-0.431193976914977,
2.16271432920345));
#12352=CARTESIAN_POINT('Ctrl Pts',(97.503739226629,-0.357260447751076,2.17614214398164));
#12353=CARTESIAN_POINT('Ctrl Pts',(97.499667166378,-0.282956121244091,2.18576115654261));
#12354=CARTESIAN_POINT('Ctrl Pts',(97.4965290156597,-0.225693172952624,
2.19317408987755));
#12355=CARTESIAN_POINT('Ctrl Pts',(97.4933908649415,-0.168210195148379,
2.1983260032933));
#12356=CARTESIAN_POINT('Ctrl Pts',(97.4902527142232,-0.110699139461686,
2.2012182310081));
#12357=CARTESIAN_POINT('Ctrl Pts',(97.4882534252855,-0.074059338587481,
2.20306084450716));
#12358=CARTESIAN_POINT('Ctrl Pts',(97.4862541363478,-0.0373731498197366,
2.20398871022549));
#12359=CARTESIAN_POINT('Ctrl Pts',(97.48425484741,-0.000671828267138261,
2.20399989760589));
#12360=CARTESIAN_POINT('',(96.7342548474632,-0.00162714762935965,2.20399939936258));
#12361=CARTESIAN_POINT('Ctrl Pts',(97.484254847371,-0.000671827551214084,
2.20399989760611));
#12362=CARTESIAN_POINT('Ctrl Pts',(97.4802137118767,0.0735120537378061,
2.20402251048162));
#12363=CARTESIAN_POINT('Ctrl Pts',(97.4761725763824,0.147847596217428,2.20029545639483));
#12364=CARTESIAN_POINT('Ctrl Pts',(97.472131440888,0.221920597882872,2.19279895299029));
#12365=CARTESIAN_POINT('Ctrl Pts',(97.4679218807762,0.299080780611764,2.18499001370719));
#12366=CARTESIAN_POINT('Ctrl Pts',(97.4637123206643,0.375955535407559,2.17309042861314));
#12367=CARTESIAN_POINT('Ctrl Pts',(97.4595027605525,0.452074506096688,2.15713806719399));
#12368=CARTESIAN_POINT('Ctrl Pts',(97.4554719719984,0.524960857081313,2.14186317050394));
#12369=CARTESIAN_POINT('Ctrl Pts',(97.4514411834444,0.597153779759007,2.12287284391787));
#12370=CARTESIAN_POINT('Ctrl Pts',(97.4474103948903,0.66824595962738,2.10025316032179));
#12371=CARTESIAN_POINT('Ctrl Pts',(97.4433818694975,0.739298223468306,2.07764617696803));
#12372=CARTESIAN_POINT('Ctrl Pts',(97.4393533441046,0.809250508664425,2.05141402580155));
#12373=CARTESIAN_POINT('Ctrl Pts',(97.4353248187118,0.87770894713221,2.0216931033478));
#12374=CARTESIAN_POINT('Ctrl Pts',(97.4312972029413,0.946151928001575,1.99197889174073));
#12375=CARTESIAN_POINT('Ctrl Pts',(97.4272695871709,1.01310128658206,1.95877766627834));
#12376=CARTESIAN_POINT('Ctrl Pts',(97.4232419714004,1.07818310152526,1.92227396579816));
#12377=CARTESIAN_POINT('Ctrl Pts',(97.4192139130876,1.14327206746455,1.88576625440003));
#12378=CARTESIAN_POINT('Ctrl Pts',(97.4151858547747,1.2064926603659,1.84595558777702));
#12379=CARTESIAN_POINT('Ctrl Pts',(97.4111577964618,1.26749705217653,1.80307160776377));
#12380=CARTESIAN_POINT('Ctrl Pts',(97.4071254264789,1.32856674363935,1.76014172435084));
#12381=CARTESIAN_POINT('Ctrl Pts',(97.403093056496,1.38741510392216,1.71413224480025));
#12382=CARTESIAN_POINT('Ctrl Pts',(97.3990606865131,1.44372549513439,1.66531459331231));
#12383=CARTESIAN_POINT('Ctrl Pts',(97.3950257630346,1.50007154486423,1.6164660280792));
#12384=CARTESIAN_POINT('Ctrl Pts',(97.3909908395561,1.55387607957638,1.56480609054044));
#12385=CARTESIAN_POINT('Ctrl Pts',(97.3869559160777,1.60485955438531,1.51064284683646));
#12386=CARTESIAN_POINT('Ctrl Pts',(97.382914382503,1.65592655139059,1.45639087177213));
#12387=CARTESIAN_POINT('Ctrl Pts',(97.3788728489284,1.70416295767579,1.39962778046808));
#12388=CARTESIAN_POINT('Ctrl Pts',(97.3748313153537,1.74933026441019,1.34069371074029));
#12389=CARTESIAN_POINT('Ctrl Pts',(97.3735882096371,1.76322294553387,1.32256661179982));
#12390=CARTESIAN_POINT('Ctrl Pts',(97.3723451039206,1.77682558613733,1.30423431700571));
#12391=CARTESIAN_POINT('Ctrl Pts',(97.371101998204,1.79013210898306,1.28570721098851));
#12392=CARTESIAN_POINT('Ctrl Pts',(97.3670289332697,1.83373124208839,1.22500271510592));
#12393=CARTESIAN_POINT('Ctrl Pts',(97.3629558683354,1.87432316218437,1.16196093021885));
#12394=CARTESIAN_POINT('Ctrl Pts',(97.3588828034011,1.91164843376739,1.09691215039068));
#12395=CARTESIAN_POINT('Ctrl Pts',(97.3548157225978,1.94891886720835,1.03195893997371));
#12396=CARTESIAN_POINT('Ctrl Pts',(97.3507486417945,1.98293194514319,0.965004999616546));
#12397=CARTESIAN_POINT('Ctrl Pts',(97.3466815609911,2.01347049427321,0.896410937400477));
#12398=CARTESIAN_POINT('Ctrl Pts',(97.342619238624,2.04397331366349,0.827897129422442));
#12399=CARTESIAN_POINT('Ctrl Pts',(97.3385569162569,2.07100948757194,0.757747446041395));
#12400=CARTESIAN_POINT('Ctrl Pts',(97.3344945938898,2.09440771754225,0.686347078889013));
#12401=CARTESIAN_POINT('Ctrl Pts',(97.3304348497523,2.11779109738413,0.61499202732774));
#12402=CARTESIAN_POINT('Ctrl Pts',(97.3263751056148,2.13754096672106,0.542388319715484));
#12403=CARTESIAN_POINT('Ctrl Pts',(97.3223153614773,2.15353463151827,0.468939858458917));
#12404=CARTESIAN_POINT('Ctrl Pts',(97.318256882024,2.16952331399747,0.395514277736344));
#12405=CARTESIAN_POINT('Ctrl Pts',(97.3141984025708,2.18175801365045,0.321244932078565));
#12406=CARTESIAN_POINT('Ctrl Pts',(97.3101399231176,2.19016667883116,0.246548005341155));
#12407=CARTESIAN_POINT('Ctrl Pts',(97.306081396487,2.19857544175739,0.171850210298192));
#12408=CARTESIAN_POINT('Ctrl Pts',(97.3020228698564,2.20315803027515,0.0967252989712811));
#12409=CARTESIAN_POINT('Ctrl Pts',(97.2979643432259,2.20389420162738,0.0215950928043276));
#12410=CARTESIAN_POINT('Ctrl Pts',(97.2939016662426,2.20463112580718,-0.0536119434247664));
#12411=CARTESIAN_POINT('Ctrl Pts',(97.2898389892594,2.2015137732694,-0.128823806808176));
#12412=CARTESIAN_POINT('Ctrl Pts',(97.2857763122762,2.19457406782218,-0.203618910817236));
#12413=CARTESIAN_POINT('Ctrl Pts',(97.281711513301,2.18763073767159,-0.278453081335427));
#12414=CARTESIAN_POINT('Ctrl Pts',(97.2776467143258,2.1768611472908,-0.352869586014872));
#12415=CARTESIAN_POINT('Ctrl Pts',(97.2735819153506,2.16234878396153,-0.426454846965158));
#12416=CARTESIAN_POINT('Ctrl Pts',(97.2695098551105,2.14781049607461,-0.500171558961478));
#12417=CARTESIAN_POINT('Ctrl Pts',(97.2654377948703,2.12951619687854,-0.573053597444631));
#12418=CARTESIAN_POINT('Ctrl Pts',(97.2613657346302,2.10759977559415,-0.644700849941666));
#12419=CARTESIAN_POINT('Ctrl Pts',(97.2582275838151,2.09070979085379,-0.69991611459003));
#12420=CARTESIAN_POINT('Ctrl Pts',(97.255089433,2.071669640917,-0.754398293751397));
#12421=CARTESIAN_POINT('Ctrl Pts',(97.2519512821849,2.05055979033752,-0.807973109856357));
#12422=CARTESIAN_POINT('Ctrl Pts',(97.2478782172477,2.02316091842555,-0.877508870833944));
#12423=CARTESIAN_POINT('Ctrl Pts',(97.2438051523106,1.99216819889427,-0.945783477852407));
#12424=CARTESIAN_POINT('Ctrl Pts',(97.2397320873735,1.95771867451018,-1.01239991676911));
#12425=CARTESIAN_POINT('Ctrl Pts',(97.2356650065672,1.92331976323126,-1.07891848307687));
#12426=CARTESIAN_POINT('Ctrl Pts',(97.231597925761,1.8854743479383,-1.14378329749517));
#12427=CARTESIAN_POINT('Ctrl Pts',(97.2275308449548,1.84436784868453,-1.20661644226275));
#12428=CARTESIAN_POINT('Ctrl Pts',(97.2234685225848,1.80330944354594,-1.26937607299831));
#12429=CARTESIAN_POINT('Ctrl Pts',(97.2194062002147,1.75899779491425,-1.33010835915344));
#12430=CARTESIAN_POINT('Ctrl Pts',(97.2153438778446,1.71166384110568,-1.388460620634));
#12431=CARTESIAN_POINT('Ctrl Pts',(97.2112841337041,1.66435992868409,-1.4467758477507));
#12432=CARTESIAN_POINT('Ctrl Pts',(97.2072243895636,1.6140378174979,-1.5027136778072));
#12433=CARTESIAN_POINT('Ctrl Pts',(97.2031646454231,1.56097050703468,-1.55595214456226));
#12434=CARTESIAN_POINT('Ctrl Pts',(97.1991061659669,1.50791972800526,-1.60917402656522));
#12435=CARTESIAN_POINT('Ctrl Pts',(97.1950476865106,1.45212578447304,-1.65969787690115));
#12436=CARTESIAN_POINT('Ctrl Pts',(97.1909892070544,1.39389943749807,-1.70723763962214));
#12437=CARTESIAN_POINT('Ctrl Pts',(97.1869306804208,1.33567241367731,-1.75477795496389));
#12438=CARTESIAN_POINT('Ctrl Pts',(97.1828721537871,1.27501330125152,-1.79933381323925));
#12439=CARTESIAN_POINT('Ctrl Pts',(97.1788136271535,1.21226567076068,-1.84065964901042));
#12440=CARTESIAN_POINT('Ctrl Pts',(97.1747509501672,1.14945387294469,-1.88202774563384));
#12441=CARTESIAN_POINT('Ctrl Pts',(97.1706882731809,1.08454969168412,-1.92015896044332));
#12442=CARTESIAN_POINT('Ctrl Pts',(97.1666255961946,1.01792476498994,-1.95485170097892));
#12443=CARTESIAN_POINT('Ctrl Pts',(97.1625607972163,0.95126503918211,-1.98956256200907));
#12444=CARTESIAN_POINT('Ctrl Pts',(97.1584959982381,0.882883212752135,-2.02083117354383));
#12445=CARTESIAN_POINT('Ctrl Pts',(97.1544311992598,0.81317213064539,-2.04850362116879));
#12446=CARTESIAN_POINT('Ctrl Pts',(97.1503591390166,0.74333651823827,-2.0762255022283));
#12447=CARTESIAN_POINT('Ctrl Pts',(97.1462870787733,0.672167360052406,-2.10033823428516));
#12448=CARTESIAN_POINT('Ctrl Pts',(97.1422150185301,0.600073492233046,-2.12073756130249));
#12449=CARTESIAN_POINT('Ctrl Pts',(97.139076867742,0.544514042076541,-2.13645839064523));
#12450=CARTESIAN_POINT('Ctrl Pts',(97.1359387169538,0.488405742393722,-2.14997481786457));
#12451=CARTESIAN_POINT('Ctrl Pts',(97.1328005661657,0.431938669814331,-2.16126004578788));
#12452=CARTESIAN_POINT('Ctrl Pts',(97.1287275012299,0.358648994181453,-2.17590735538197));
#12453=CARTESIAN_POINT('Ctrl Pts',(97.1246544362941,0.284472090730599,-2.18685073776327));
#12454=CARTESIAN_POINT('Ctrl Pts',(97.1205813713583,0.209815900133298,-2.19399026617058));
#12455=CARTESIAN_POINT('Ctrl Pts',(97.1165142905535,0.135269394116645,-2.20111930521093));
#12456=CARTESIAN_POINT('Ctrl Pts',(97.1124472097486,0.0602454703586018,
-2.20445554086714));
#12457=CARTESIAN_POINT('Ctrl Pts',(97.1083801289437,-0.0148377690601739,
-2.20395005401877));
#12458=CARTESIAN_POINT('Ctrl Pts',(97.1043178065751,-0.0898331619814498,
-2.20344515858399));
#12459=CARTESIAN_POINT('Ctrl Pts',(97.1002554842064,-0.164887257633621,
-2.19910747392425));
#12460=CARTESIAN_POINT('Ctrl Pts',(97.0961931618377,-0.239578503319732,
-2.19094001304168));
#12461=CARTESIAN_POINT('Ctrl Pts',(97.0921334176986,-0.314222344797098,
-2.18277773579231));
#12462=CARTESIAN_POINT('Ctrl Pts',(97.0880736735595,-0.388503319864604,
-2.17079055743129));
#12463=CARTESIAN_POINT('Ctrl Pts',(97.0840139294204,-0.462002901034642,
-2.15503348452769));
#12464=CARTESIAN_POINT('Ctrl Pts',(97.0799554499655,-0.535479585746291,
-2.13928132023934));
#12465=CARTESIAN_POINT('Ctrl Pts',(97.0758969705107,-0.608174893309045,
-2.11976169313124));
#12466=CARTESIAN_POINT('Ctrl Pts',(97.0718384910558,-0.679680018633716,
-2.09658080508958));
#12467=CARTESIAN_POINT('Ctrl Pts',(97.0677799644236,-0.751185975161896,
-2.07339964758422));
#12468=CARTESIAN_POINT('Ctrl Pts',(97.0637214377914,-0.821501268344636,
-2.0465572935882));
#12469=CARTESIAN_POINT('Ctrl Pts',(97.0596629111592,-0.890233348282234,
-2.01620945975516));
#12470=CARTESIAN_POINT('Ctrl Pts',(97.0556002341743,-0.959035715395272,
-1.98583059145434));
#12471=CARTESIAN_POINT('Ctrl Pts',(97.0515375571894,-1.02625119839503,-1.95193927797258));
#12472=CARTESIAN_POINT('Ctrl Pts',(97.0474748802044,-1.09150899888306,-1.91473865197246));
#12473=CARTESIAN_POINT('Ctrl Pts',(97.0434100812276,-1.15680088441586,-1.87751859557485));
#12474=CARTESIAN_POINT('Ctrl Pts',(97.0393452822508,-1.22013264865409,-1.83698604213826));
#12475=CARTESIAN_POINT('Ctrl Pts',(97.0352804832739,-1.28116207596802,-1.79338778157467));
#12476=CARTESIAN_POINT('Ctrl Pts',(97.0312084230321,-1.34230052487086,-1.74971163806429));
#12477=CARTESIAN_POINT('Ctrl Pts',(97.0271363627902,-1.40112804741936,-1.70295914603113));
#12478=CARTESIAN_POINT('Ctrl Pts',(97.0230643025484,-1.45733550120218,-1.65341744182641));
#12479=CARTESIAN_POINT('Ctrl Pts',(97.0199261517478,-1.50065201805453,-1.61523791365619));
#12480=CARTESIAN_POINT('Ctrl Pts',(97.0167880009472,-1.54241312561684,-1.57540269030054));
#12481=CARTESIAN_POINT('Ctrl Pts',(97.0136498501466,-1.58249331359919,-1.53405701080952));
#12482=CARTESIAN_POINT('Ctrl Pts',(97.0095767852108,-1.63451414327371,-1.48039367590884));
#12483=CARTESIAN_POINT('Ctrl Pts',(97.005503720275,-1.68390256182177,-1.42397776736522));
#12484=CARTESIAN_POINT('Ctrl Pts',(97.0014306553391,-1.73035355074903,-1.36509801457999));
#12485=CARTESIAN_POINT('Ctrl Pts',(96.9973635745343,-1.77673629406656,-1.30630476769532));
#12486=CARTESIAN_POINT('Ctrl Pts',(96.9932964937294,-1.82018988283804,-1.2450552352296));
#12487=CARTESIAN_POINT('Ctrl Pts',(96.9892294129245,-1.86044666453567,-1.18167432417655));
#12488=CARTESIAN_POINT('Ctrl Pts',(96.9851670905559,-1.90065634627732,-1.11836756803592));
#12489=CARTESIAN_POINT('Ctrl Pts',(96.9811047681872,-1.93767639721694,-1.05293478870622));
#12490=CARTESIAN_POINT('Ctrl Pts',(96.9770424458185,-1.9712809438603,-0.985731931294325));
#12491=CARTESIAN_POINT('Ctrl Pts',(96.9729827016794,-2.00486416274382,-0.918571725444404));
#12492=CARTESIAN_POINT('Ctrl Pts',(96.9689229575403,-2.03503596592421,-0.849644096768522));
#12493=CARTESIAN_POINT('Ctrl Pts',(96.9648632134011,-2.06161581931966,-0.779330618884511));
#12494=CARTESIAN_POINT('Ctrl Pts',(96.9608047339463,-2.08818739260662,-0.709039044929665));
#12495=CARTESIAN_POINT('Ctrl Pts',(96.9567462544914,-2.11116906903231,-0.637362925246967));
#12496=CARTESIAN_POINT('Ctrl Pts',(96.9526877750366,-2.13042861167752,-0.564703400508454));
#12497=CARTESIAN_POINT('Ctrl Pts',(96.9486292484044,-2.14968837820304,-0.492043031147718));
#12498=CARTESIAN_POINT('Ctrl Pts',(96.9445707217722,-2.16522580443817,-0.418399696015615));
#12499=CARTESIAN_POINT('Ctrl Pts',(96.94051219514,-2.17695907773433,-0.344187701509047));
#12500=CARTESIAN_POINT('Ctrl Pts',(96.9364495181551,-2.18870434977464,-0.269899815926551));
#12501=CARTESIAN_POINT('Ctrl Pts',(96.9323868411702,-2.19663762559302,-0.195042582346671));
#12502=CARTESIAN_POINT('Ctrl Pts',(96.9283241641853,-2.2007287308317,-0.120037716122496));
#12503=CARTESIAN_POINT('Ctrl Pts',(96.9242593652085,-2.20482197291079,-0.0449936738274561));
#12504=CARTESIAN_POINT('Ctrl Pts',(96.9201945662316,-2.20506904645644,0.0301976767676627));
#12505=CARTESIAN_POINT('Ctrl Pts',(96.9161297672548,-2.20149195750705,0.105114989567421));
#12506=CARTESIAN_POINT('Ctrl Pts',(96.912057707013,-2.19790847852686,0.18016613296061));
#12507=CARTESIAN_POINT('Ctrl Pts',(96.9079856467712,-2.19048723909058,0.254941784918909));
#12508=CARTESIAN_POINT('Ctrl Pts',(96.9039135865294,-2.1793020759338,0.329026536666328));
#12509=CARTESIAN_POINT('Ctrl Pts',(96.9007754357287,-2.17068218167106,0.386120270355525));
#12510=CARTESIAN_POINT('Ctrl Pts',(96.8976372849281,-2.15982793250988,0.442803781184796));
#12511=CARTESIAN_POINT('Ctrl Pts',(96.8944991341274,-2.14679339697907,0.498892884983425));
#12512=CARTESIAN_POINT('Ctrl Pts',(96.8904260691913,-2.12987562820314,0.57169198754225));
#12513=CARTESIAN_POINT('Ctrl Pts',(96.8863530042551,-2.10921804283281,0.643769964700029));
#12514=CARTESIAN_POINT('Ctrl Pts',(96.882279939319,-2.08489805097604,0.714714010661834));
#12515=CARTESIAN_POINT('Ctrl Pts',(96.8782128585138,-2.06061378995533,0.78555382591126));
#12516=CARTESIAN_POINT('Ctrl Pts',(96.8741457777086,-2.03267795906397,0.855262569679648));
#12517=CARTESIAN_POINT('Ctrl Pts',(96.8700786969034,-2.00121862111457,0.923439240288346));
#12518=CARTESIAN_POINT('Ctrl Pts',(96.8660163745344,-1.9697960902165,0.991536145003068));
#12519=CARTESIAN_POINT('Ctrl Pts',(96.8619540521654,-1.934858441693,1.05810410650828));
#12520=CARTESIAN_POINT('Ctrl Pts',(96.8578917297963,-1.89658246244903,1.12276042107423));
#12521=CARTESIAN_POINT('Ctrl Pts',(96.8538319856569,-1.85833077577774,1.18737570028976));
#12522=CARTESIAN_POINT('Ctrl Pts',(96.8497722415174,-1.81674520539716,1.25008133033255));
#12523=CARTESIAN_POINT('Ctrl Pts',(96.845712497378,-1.77204864465173,1.31051882893302));
#12524=CARTESIAN_POINT('Ctrl Pts',(96.8416540179228,-1.72736600769908,1.37093750015187));
#12525=CARTESIAN_POINT('Ctrl Pts',(96.8375955384676,-1.67957458826537,1.4290890591465));
#12526=CARTESIAN_POINT('Ctrl Pts',(96.8335370590124,-1.62893989408494,1.48464501530115));
#12527=CARTESIAN_POINT('Ctrl Pts',(96.8294785323798,-1.57830461130708,1.5402016172599));
#12528=CARTESIAN_POINT('Ctrl Pts',(96.8254200057472,-1.52482631110719,1.59316220479494));
#12529=CARTESIAN_POINT('Ctrl Pts',(96.8213614791147,-1.46880888784006,1.64323353513797));
#12530=CARTESIAN_POINT('Ctrl Pts',(96.8172988021294,-1.41273417972928,1.69335606969862));
#12531=CARTESIAN_POINT('Ctrl Pts',(96.8132361251442,-1.35411552011598,1.74058312794341));
#12532=CARTESIAN_POINT('Ctrl Pts',(96.8091734481589,-1.29329100922578,1.78466085446389));
#12533=CARTESIAN_POINT('Ctrl Pts',(96.8051086491817,-1.23243472885871,1.82876160338589));
#12534=CARTESIAN_POINT('Ctrl Pts',(96.8010438502045,-1.16937070365075,1.86970948459025));
#12535=CARTESIAN_POINT('Ctrl Pts',(96.7969790512273,-1.10446499587837,1.90729470006064));
#12536=CARTESIAN_POINT('Ctrl Pts',(96.7929069909851,-1.03944334201756,1.9449470569099));
#12537=CARTESIAN_POINT('Ctrl Pts',(96.788834930743,-0.972573859713514,1.97922453140597));
#12538=CARTESIAN_POINT('Ctrl Pts',(96.7847628705008,-0.904245703895851,
2.0099641058949));
#12539=CARTESIAN_POINT('Ctrl Pts',(96.7816247197033,-0.851588315763736,
2.03365369162292));
#12540=CARTESIAN_POINT('Ctrl Pts',(96.7784865689059,-0.798065098219529,
2.05524304783608));
#12541=CARTESIAN_POINT('Ctrl Pts',(96.7753484181084,-0.743860152430341,
2.07467782405517));
#12542=CARTESIAN_POINT('Ctrl Pts',(96.7706169458065,-0.662133933335203,
2.103980146126));
#12543=CARTESIAN_POINT('Ctrl Pts',(96.7658854735045,-0.578598797540645,
2.12847663192413));
#12544=CARTESIAN_POINT('Ctrl Pts',(96.7611540012026,-0.493786047533441,
2.14797377527318));
#12545=CARTESIAN_POINT('Ctrl Pts',(96.7564655031284,-0.409743620629903,
2.16729383321967));
#12546=CARTESIAN_POINT('Ctrl Pts',(96.7517770050542,-0.324446834544995,
2.18170486705532));
#12547=CARTESIAN_POINT('Ctrl Pts',(96.7470885069799,-0.238433665781087,
2.19106489794853));
#12548=CARTESIAN_POINT('Ctrl Pts',(96.7428106204744,-0.159953400218962,
2.19960519149573));
#12549=CARTESIAN_POINT('Ctrl Pts',(96.7385327339688,-0.080877055221892,
2.2039408914976));
#12550=CARTESIAN_POINT('Ctrl Pts',(96.7342548474632,-0.00162714762936041,
2.20399939936258));
#12551=CARTESIAN_POINT('',(95.9842548473824,0.00150560105777076,2.20399948574528));
#12552=CARTESIAN_POINT('Ctrl Pts',(96.73425484741,-0.00162714664304999,
2.2039993993633));
#12553=CARTESIAN_POINT('Ctrl Pts',(96.7301906605558,0.0736638719990596,
2.20405498446386));
#12554=CARTESIAN_POINT('Ctrl Pts',(96.7261264737017,0.148992315837502,2.20024821452564));
#12555=CARTESIAN_POINT('Ctrl Pts',(96.7220622868475,0.223934505578098,2.19259420258549));
#12556=CARTESIAN_POINT('Ctrl Pts',(96.7179984623146,0.298870014240871,2.18494087299862));
#12557=CARTESIAN_POINT('Ctrl Pts',(96.7139346377817,0.373418864702078,2.1734410315032));
#12558=CARTESIAN_POINT('Ctrl Pts',(96.7098708132488,0.447162387060237,2.15816167133016));
#12559=CARTESIAN_POINT('Ctrl Pts',(96.7058060546237,0.520922859768338,2.14287879911303));
#12560=CARTESIAN_POINT('Ctrl Pts',(96.7017412959986,0.593877172113965,2.12381478140672));
#12561=CARTESIAN_POINT('Ctrl Pts',(96.6976765373735,0.665618288343953,2.10108740756354));
#12562=CARTESIAN_POINT('Ctrl Pts',(96.6936067811457,0.737447609957902,2.0783320905151));
#12563=CARTESIAN_POINT('Ctrl Pts',(96.689537024918,0.808060305621242,2.0519045738805));
#12564=CARTESIAN_POINT('Ctrl Pts',(96.6854672686902,0.877066608908877,2.02197185033251));
#12565=CARTESIAN_POINT('Ctrl Pts',(96.681394634172,0.946121716147331,1.99201795719423));
#12566=CARTESIAN_POINT('Ctrl Pts',(96.6773219996537,1.01356774536582,1.9585541355077));
#12567=CARTESIAN_POINT('Ctrl Pts',(96.6732493651355,1.07903933529307,1.92179346259953));
#12568=CARTESIAN_POINT('Ctrl Pts',(96.6691695124382,1.14462696452116,1.88496763650374));
#12569=CARTESIAN_POINT('Ctrl Pts',(96.6650896597409,1.20823277037885,1.84483355202713));
#12570=CARTESIAN_POINT('Ctrl Pts',(96.6610098070436,1.26952072280493,1.80164733906746));
#12571=CARTESIAN_POINT('Ctrl Pts',(96.6594057720588,1.29361669565812,1.78466824653922));
#12572=CARTESIAN_POINT('Ctrl Pts',(96.657801737074,1.31735475748164,1.76721780370166));
#12573=CARTESIAN_POINT('Ctrl Pts',(96.6561977020891,1.34071599508255,1.74931318537585));
#12574=CARTESIAN_POINT('Ctrl Pts',(96.6521246371532,1.40003629584514,1.70384867008471));
#12575=CARTESIAN_POINT('Ctrl Pts',(96.6480515722172,1.45715577536579,1.65527567673152));
#12576=CARTESIAN_POINT('Ctrl Pts',(96.6439785072812,1.51173041220667,1.6038351414062));
#12577=CARTESIAN_POINT('Ctrl Pts',(96.6399114264762,1.56622486820639,1.55247018231247));
#12578=CARTESIAN_POINT('Ctrl Pts',(96.6358443456711,1.61818156015399,1.49824637050675));
#12579=CARTESIAN_POINT('Ctrl Pts',(96.6317772648661,1.66728813025811,1.44144590280052));
#12580=CARTESIAN_POINT('Ctrl Pts',(96.6277149424972,1.71633724625903,1.38471189096622));
#12581=CARTESIAN_POINT('Ctrl Pts',(96.6236526201284,1.76254255482621,1.32540757204212));
#12582=CARTESIAN_POINT('Ctrl Pts',(96.6195902977596,1.80562848010989,1.26385196594223));
#12583=CARTESIAN_POINT('Ctrl Pts',(96.6155305536203,1.84868706009789,1.20233542726956));
#12584=CARTESIAN_POINT('Ctrl Pts',(96.611470809481,1.88862991235382,1.1385708269324));
#12585=CARTESIAN_POINT('Ctrl Pts',(96.6074110653417,1.9252225573414,1.07290917821773));
#12586=CARTESIAN_POINT('Ctrl Pts',(96.6033525858867,1.96180380305348,1.00726798430276));
#12587=CARTESIAN_POINT('Ctrl Pts',(96.5992941064317,1.99503668134416,0.93973133214225));
#12588=CARTESIAN_POINT('Ctrl Pts',(96.5952356269766,2.02473162271737,0.870676665570101));
#12589=CARTESIAN_POINT('Ctrl Pts',(96.5911771003443,2.0544269092761,0.801621196279736));
#12590=CARTESIAN_POINT('Ctrl Pts',(96.5871185737119,2.08058399028871,0.731048116874426));
#12591=CARTESIAN_POINT('Ctrl Pts',(96.5830600470795,2.10306124812793,0.659355281030354));
#12592=CARTESIAN_POINT('Ctrl Pts',(96.5789973700945,2.12556149178352,0.58758913026626));
#12593=CARTESIAN_POINT('Ctrl Pts',(96.5749346931094,2.14437425445206,0.514701392987236));
#12594=CARTESIAN_POINT('Ctrl Pts',(96.5708720161243,2.15940791454958,0.441104815866537));
#12595=CARTESIAN_POINT('Ctrl Pts',(96.5668072171473,2.17444942693409,0.367469798243549));
#12596=CARTESIAN_POINT('Ctrl Pts',(96.5627424181703,2.1857078344072,0.293125676005957));
#12597=CARTESIAN_POINT('Ctrl Pts',(96.5586776191932,2.19314318703594,0.218492473915826));
#12598=CARTESIAN_POINT('Ctrl Pts',(96.5546055589513,2.20059182201046,0.143725948761373));
#12599=CARTESIAN_POINT('Ctrl Pts',(96.5505334987093,2.20420373792287,0.0686697898906166));
#12600=CARTESIAN_POINT('Ctrl Pts',(96.5464614384673,2.20399112617167,-0.0062542590722837));
#12601=CARTESIAN_POINT('Ctrl Pts',(96.5433232876682,2.20382727600805,-0.0639948007512024));
#12602=CARTESIAN_POINT('Ctrl Pts',(96.5401851368692,2.20139308210989,-0.12165683177191));
#12603=CARTESIAN_POINT('Ctrl Pts',(96.5370469860701,2.19671505058251,-0.179050234694871));
#12604=CARTESIAN_POINT('Ctrl Pts',(96.5329739211341,2.19064334549127,-0.253542211649531));
#12605=CARTESIAN_POINT('Ctrl Pts',(96.5289008561981,2.18076653246242,-0.327868648322466));
#12606=CARTESIAN_POINT('Ctrl Pts',(96.5248277912621,2.16710071900694,-0.401609852567912));
#12607=CARTESIAN_POINT('Ctrl Pts',(96.520760710457,2.15345498331064,-0.475242716527136));
#12608=CARTESIAN_POINT('Ctrl Pts',(96.5166936296519,2.13603138580631,-0.548291589584893));
#12609=CARTESIAN_POINT('Ctrl Pts',(96.5126265488468,2.11489786941609,-0.620341036800958));
#12610=CARTESIAN_POINT('Ctrl Pts',(96.5085642264779,2.0937890789888,-0.692306187020324));
#12611=CARTESIAN_POINT('Ctrl Pts',(96.504501904109,2.06897912709108,-0.763273778706842));
#12612=CARTESIAN_POINT('Ctrl Pts',(96.5004395817402,2.04058683546056,-0.832839340416293));
#12613=CARTESIAN_POINT('Ctrl Pts',(96.4963798376008,2.0122125635338,-0.902360751029051));
#12614=CARTESIAN_POINT('Ctrl Pts',(96.4923200934615,1.9802606435506,-0.9704814564863));
#12615=CARTESIAN_POINT('Ctrl Pts',(96.4882603493221,1.94489905431959,-1.03681419189109));
#12616=CARTESIAN_POINT('Ctrl Pts',(96.4842018698671,1.9095484808678,-1.10312626344042));
#12617=CARTESIAN_POINT('Ctrl Pts',(96.480143390412,1.87079057153174,-1.16765104975184));
#12618=CARTESIAN_POINT('Ctrl Pts',(96.4760849109569,1.82883985302339,-1.23002471194418));
#12619=CARTESIAN_POINT('Ctrl Pts',(96.4720263843245,1.78688864686362,-1.29239909919216));
#12620=CARTESIAN_POINT('Ctrl Pts',(96.4679678576921,1.74174482579206,-1.35262191748397));
#12621=CARTESIAN_POINT('Ctrl Pts',(96.4639093310597,1.6936660521818,-1.41035857273494));
#12622=CARTESIAN_POINT('Ctrl Pts',(96.4598466540746,1.64553811199305,-1.46815427096014));
#12623=CARTESIAN_POINT('Ctrl Pts',(96.4557839770894,1.59446953193652,-1.5234583613693));
#12624=CARTESIAN_POINT('Ctrl Pts',(96.4517213001043,1.54075758074572,-1.57597020193105));
#12625=CARTESIAN_POINT('Ctrl Pts',(96.4476565011272,1.48701757506562,-1.62850947014785));
#12626=CARTESIAN_POINT('Ctrl Pts',(96.4435917021502,1.43063180716094,-1.67825326803271));
#12627=CARTESIAN_POINT('Ctrl Pts',(96.4395269031731,1.37193165971791,-1.72494043985978));
#12628=CARTESIAN_POINT('Ctrl Pts',(96.4354548429311,1.31312665165904,-1.77171101259474));
#12629=CARTESIAN_POINT('Ctrl Pts',(96.431382782689,1.25199939498887,-1.81541377467077));
#12630=CARTESIAN_POINT('Ctrl Pts',(96.427310722447,1.18891096833104,-1.85583046353436));
#12631=CARTESIAN_POINT('Ctrl Pts',(96.4241725716483,1.14029160006606,-1.88697775922724));
#12632=CARTESIAN_POINT('Ctrl Pts',(96.4210344208496,1.09050810071271,-1.9161743054736));
#12633=CARTESIAN_POINT('Ctrl Pts',(96.4178962700509,1.03973462442981,-1.94333937096993));
#12634=CARTESIAN_POINT('Ctrl Pts',(96.4138232051149,0.973834774743817,-1.97859742032909));
#12635=CARTESIAN_POINT('Ctrl Pts',(96.4097501401789,0.906012375112024,-2.01056760538032));
#12636=CARTESIAN_POINT('Ctrl Pts',(96.4056770752429,0.836628901732491,-2.0390360665731));
#12637=CARTESIAN_POINT('Ctrl Pts',(96.4016099944379,0.767347366278208,-2.06746270201505));
#12638=CARTESIAN_POINT('Ctrl Pts',(96.3975429136328,0.696509748712963,-2.09239764822724));
#12639=CARTESIAN_POINT('Ctrl Pts',(96.3934758328278,0.624502032568093,-2.11367291966338));
#12640=CARTESIAN_POINT('Ctrl Pts',(96.3894135104589,0.552578564595041,-2.13492329928487));
#12641=CARTESIAN_POINT('Ctrl Pts',(96.3853511880901,0.479488173527562,-2.15252237643355));
#12642=CARTESIAN_POINT('Ctrl Pts',(96.3812888657212,0.405635195328789,-2.16635086916007));
#12643=CARTESIAN_POINT('Ctrl Pts',(96.3772291215819,0.331829089316586,-2.18017058537267));
#12644=CARTESIAN_POINT('Ctrl Pts',(96.3731693774426,0.257261824714813,-2.19022437830546));
#12645=CARTESIAN_POINT('Ctrl Pts',(96.3691096333033,0.182349909793452,-2.1964436051031));
#12646=CARTESIAN_POINT('Ctrl Pts',(96.3650511538482,0.107461331298148,-2.20266089449831));
#12647=CARTESIAN_POINT('Ctrl Pts',(96.3609926743932,0.0322287911648629,
-2.2050459499835));
#12648=CARTESIAN_POINT('Ctrl Pts',(96.3569341949382,-0.0429256711574192,
-2.20358194464279));
#12649=CARTESIAN_POINT('Ctrl Pts',(96.3528756683058,-0.118081007104319,
-2.20211792228391));
#12650=CARTESIAN_POINT('Ctrl Pts',(96.3488171416734,-0.193157786102896,
-2.19680476135209));
#12651=CARTESIAN_POINT('Ctrl Pts',(96.344758615041,-0.267735176999542,-2.1876777356359));
#12652=CARTESIAN_POINT('Ctrl Pts',(96.3406959380559,-0.342388832635664,
-2.17854137639075));
#12653=CARTESIAN_POINT('Ctrl Pts',(96.3366332610708,-0.416541605379462,
-2.16558342210309));
#12654=CARTESIAN_POINT('Ctrl Pts',(96.3325705840857,-0.489779741042405,
-2.14889083139755));
#12655=CARTESIAN_POINT('Ctrl Pts',(96.3285057851087,-0.563056129988674,
-2.13218952192279));
#12656=CARTESIAN_POINT('Ctrl Pts',(96.3244409861316,-0.635416470597316,
-2.11174982140798));
#12657=CARTESIAN_POINT('Ctrl Pts',(96.3203761871546,-0.706461713050952,
-2.08770875554832));
#12658=CARTESIAN_POINT('Ctrl Pts',(96.3163041269126,-0.777633869119079,
-2.06362474327228));
#12659=CARTESIAN_POINT('Ctrl Pts',(96.3122320666706,-0.847485790065002,
-2.03592669169464));
#12660=CARTESIAN_POINT('Ctrl Pts',(96.3081600064286,-0.915638387665817,
-2.00479982617536));
#12661=CARTESIAN_POINT('Ctrl Pts',(96.3050218556296,-0.96816048112697,-1.98081177293148));
#12662=CARTESIAN_POINT('Ctrl Pts',(96.3018837048307,-1.01967373109716,-1.95478831815319));
#12663=CARTESIAN_POINT('Ctrl Pts',(96.2987455540318,-1.07001592308488,-1.92683209552488));
#12664=CARTESIAN_POINT('Ctrl Pts',(96.2946724890958,-1.13535600076876,-1.89054718844879));
#12665=CARTESIAN_POINT('Ctrl Pts',(96.2905994241598,-1.19897432457061,-1.85086495690024));
#12666=CARTESIAN_POINT('Ctrl Pts',(96.2865263592238,-1.26049529155207,-1.80797334603558));
#12667=CARTESIAN_POINT('Ctrl Pts',(96.2824592784188,-1.32192587217154,-1.76514475135638));
#12668=CARTESIAN_POINT('Ctrl Pts',(96.2783921976137,-1.38126482544665,-1.7191164097707));
#12669=CARTESIAN_POINT('Ctrl Pts',(96.2743251168087,-1.43816182669763,-1.67012172018381));
#12670=CARTESIAN_POINT('Ctrl Pts',(96.2702627944398,-1.49499225913369,-1.62118435380116));
#12671=CARTESIAN_POINT('Ctrl Pts',(96.2662004720709,-1.54938605587491,-1.56928784467997));
#12672=CARTESIAN_POINT('Ctrl Pts',(96.2621381497021,-1.60102388360845,-1.51470740544678));
#12673=CARTESIAN_POINT('Ctrl Pts',(96.2580784055628,-1.65262893841995,-1.46016160671956));
#12674=CARTESIAN_POINT('Ctrl Pts',(96.2540186614234,-1.70148116787368,-1.40293560406399));
#12675=CARTESIAN_POINT('Ctrl Pts',(96.2499589172841,-1.74729720531625,-1.34334227816071));
#12676=CARTESIAN_POINT('Ctrl Pts',(96.2459004378291,-1.79309897022865,-1.28376751666392));
#12677=CARTESIAN_POINT('Ctrl Pts',(96.241841958374,-1.83586613020979,-1.22182727439976));
#12678=CARTESIAN_POINT('Ctrl Pts',(96.237783478919,-1.87535587269699,-1.15786715591251));
#12679=CARTESIAN_POINT('Ctrl Pts',(96.2337249522866,-1.91484607422822,-1.09390629392811));
#12680=CARTESIAN_POINT('Ctrl Pts',(96.2296664256542,-1.95105853331316,-1.02792591630782));
#12681=CARTESIAN_POINT('Ctrl Pts',(96.2256078990218,-1.98379488240875,-0.960298841261847));
#12682=CARTESIAN_POINT('Ctrl Pts',(96.2215452220367,-2.01656470852874,-0.892602609046438));
#12683=CARTESIAN_POINT('Ctrl Pts',(96.2174825450516,-2.04585111751407,-0.823256747355467));
#12684=CARTESIAN_POINT('Ctrl Pts',(96.2134198680665,-2.07150301707198,-0.752656130156174));
#12685=CARTESIAN_POINT('Ctrl Pts',(96.2093550690895,-2.09716831496909,-0.682018637285601));
#12686=CARTESIAN_POINT('Ctrl Pts',(96.2052902701124,-2.1191951830527,-0.610125540728479));
#12687=CARTESIAN_POINT('Ctrl Pts',(96.2012254711354,-2.13748257724314,-0.537386482879899));
#12688=CARTESIAN_POINT('Ctrl Pts',(96.1971534108933,-2.155802639621,-0.464517485623342));
#12689=CARTESIAN_POINT('Ctrl Pts',(96.1930813506513,-2.17036979240415,-0.390799977656557));
#12690=CARTESIAN_POINT('Ctrl Pts',(96.1890092904093,-2.18113431865364,-0.316652939337917));
#12691=CARTESIAN_POINT('Ctrl Pts',(96.1858711396104,-2.18943004726324,-0.259511204268338));
#12692=CARTESIAN_POINT('Ctrl Pts',(96.1827329888115,-2.19546842055734,-0.202114573975238));
#12693=CARTESIAN_POINT('Ctrl Pts',(96.1795948380126,-2.19924781041177,-0.144654997836399));
#12694=CARTESIAN_POINT('Ctrl Pts',(96.1755217730766,-2.20415315157665,-0.0700771334172606));
#12695=CARTESIAN_POINT('Ctrl Pts',(96.1714487081406,-2.20527017959899,0.00489434697652635));
#12696=CARTESIAN_POINT('Ctrl Pts',(96.1673756432046,-2.20255335191165,0.0798419187065264));
#12697=CARTESIAN_POINT('Ctrl Pts',(96.1633085623996,-2.19984051577682,0.154679377760128));
#12698=CARTESIAN_POINT('Ctrl Pts',(96.1592414815945,-2.19330502426454,0.229492524704092));
#12699=CARTESIAN_POINT('Ctrl Pts',(96.1551744007894,-2.18295323469984,0.303860453355697));
#12700=CARTESIAN_POINT('Ctrl Pts',(96.1511120784206,-2.17261355660587,0.378141372414798));
#12701=CARTESIAN_POINT('Ctrl Pts',(96.1470497560517,-2.15846651693741,0.4519776375663));
#12702=CARTESIAN_POINT('Ctrl Pts',(96.1429874336828,-2.14057040896888,0.52495173515933));
#12703=CARTESIAN_POINT('Ctrl Pts',(96.1389276895435,-2.12268565910306,0.59787951836394));
#12704=CARTESIAN_POINT('Ctrl Pts',(96.1348679454042,-2.10105667606701,0.66994575730682));
#12705=CARTESIAN_POINT('Ctrl Pts',(96.1308082012649,-2.07579290039091,0.740742758781129));
#12706=CARTESIAN_POINT('Ctrl Pts',(96.1267497218099,-2.05053699484118,0.811517705699732));
#12707=CARTESIAN_POINT('Ctrl Pts',(96.1226912423548,-2.02164870515795,0.881023750787546));
#12708=CARTESIAN_POINT('Ctrl Pts',(96.1186327628998,-1.98928694912814,0.948869555855008));
#12709=CARTESIAN_POINT('Ctrl Pts',(96.1145742362674,-1.95692481691258,1.01671614958869));
#12710=CARTESIAN_POINT('Ctrl Pts',(96.110515709635,-1.92108934535601,1.08290203480788));
#12711=CARTESIAN_POINT('Ctrl Pts',(96.1064571830025,-1.88198640639796,1.14705848418174));
#12712=CARTESIAN_POINT('Ctrl Pts',(96.1023945060174,-1.84284347977863,1.2112805415747));
#12713=CARTESIAN_POINT('Ctrl Pts',(96.0983318290323,-1.80042666222557,1.27346861015385));
#12714=CARTESIAN_POINT('Ctrl Pts',(96.0942691520472,-1.75498597811549,1.33328174690049));
#12715=CARTESIAN_POINT('Ctrl Pts',(96.0902043530702,-1.70952155971248,1.39312612486932));
#12716=CARTESIAN_POINT('Ctrl Pts',(96.0861395540932,-1.66103043771791,1.45059273550423));
#12717=CARTESIAN_POINT('Ctrl Pts',(96.0820747551161,-1.60980216643582,1.50537469918241));
#12718=CARTESIAN_POINT('Ctrl Pts',(96.0780026948741,-1.55848238212846,1.5602545241216));
#12719=CARTESIAN_POINT('Ctrl Pts',(96.0739306346321,-1.50441602602296,1.61243979080215));
#12720=CARTESIAN_POINT('Ctrl Pts',(96.0698585743901,-1.44792831102597,1.66166170026558));
#12721=CARTESIAN_POINT('Ctrl Pts',(96.0667204235912,-1.4043958096856,1.69959477721525));
#12722=CARTESIAN_POINT('Ctrl Pts',(96.0635822727924,-1.35942598893592,1.73576866756006));
#12723=CARTESIAN_POINT('Ctrl Pts',(96.0604441219935,-1.31317929896625,1.77007800075774));
#12724=CARTESIAN_POINT('Ctrl Pts',(96.0563512646815,-1.25286317162506,1.81482511912447));
#12725=CARTESIAN_POINT('Ctrl Pts',(96.0522584073694,-1.1901404740041,1.85657251872614));
#12726=CARTESIAN_POINT('Ctrl Pts',(96.0481655500574,-1.1253399084655,1.89505305741419));
#12727=CARTESIAN_POINT('Ctrl Pts',(96.044078778494,-1.06063569613981,1.93347637864577));
#12728=CARTESIAN_POINT('Ctrl Pts',(96.0399920069305,-0.993860150335465,
1.96864224341765));
#12729=CARTESIAN_POINT('Ctrl Pts',(96.0359052353671,-0.925373102248549,
2.00032512898151));
#12730=CARTESIAN_POINT('Ctrl Pts',(96.0318232633005,-0.856966485220754,
2.03197080622477));
#12731=CARTESIAN_POINT('Ctrl Pts',(96.0277412912338,-0.78685278257689,2.06014143048253));
#12732=CARTESIAN_POINT('Ctrl Pts',(96.0236593191671,-0.715417411484009,
2.0846567888613));
#12733=CARTESIAN_POINT('Ctrl Pts',(96.0195809795603,-0.644045609203774,
2.10915033154569));
#12734=CARTESIAN_POINT('Ctrl Pts',(96.0155026399535,-0.571354920030052,
2.12999492007944));
#12735=CARTESIAN_POINT('Ctrl Pts',(96.0114243003467,-0.497750332949793,
2.14705859399514));
#12736=CARTESIAN_POINT('Ctrl Pts',(96.0073480219645,-0.424182946201418,
2.16411364379707));
#12737=CARTESIAN_POINT('Ctrl Pts',(96.0032717435823,-0.349703037890821,
2.17739147084455));
#12738=CARTESIAN_POINT('Ctrl Pts',(95.9991954652001,-0.274728945169834,
2.18681046428031));
#12739=CARTESIAN_POINT('Ctrl Pts',(95.9951194772191,-0.19976019373505,2.19622878669041));
#12740=CARTESIAN_POINT('Ctrl Pts',(95.9910434892382,-0.124297794801206,
2.20178876026211));
#12741=CARTESIAN_POINT('Ctrl Pts',(95.9869675012572,-0.048767058015047,
2.20346040900502));
#12742=CARTESIAN_POINT('Ctrl Pts',(95.9860632833082,-0.0320113049980311,
2.20383124788015));
#12743=CARTESIAN_POINT('Ctrl Pts',(95.9851590653591,-0.0152522006656639,
2.20401093336839));
#12744=CARTESIAN_POINT('Ctrl Pts',(95.98425484741,0.00150560054724205,2.20399948574563));
#12745=CARTESIAN_POINT('',(95.2342548474574,0.000867116891644239,2.20399982942565));
#12746=CARTESIAN_POINT('Ctrl Pts',(95.9842548473825,0.00150560105777081,
2.20399948574528));
#12747=CARTESIAN_POINT('Ctrl Pts',(95.9796357852113,0.0871103225000559,
2.20394100725652));
#12748=CARTESIAN_POINT('Ctrl Pts',(95.9750167230401,0.172519533150872,2.19889107907991));
#12749=CARTESIAN_POINT('Ctrl Pts',(95.9703976608689,0.257195271049002,2.18894188880154));
#12750=CARTESIAN_POINT('Ctrl Pts',(95.9655469517198,0.346117515718511,2.17849374445514));
#12751=CARTESIAN_POINT('Ctrl Pts',(95.9606962425707,0.434230493468681,2.16264236725634));
#12752=CARTESIAN_POINT('Ctrl Pts',(95.9558455334216,0.520933001701834,2.14155196241836));
#12753=CARTESIAN_POINT('Ctrl Pts',(95.9509948242725,0.607635509934981,2.12046155758038));
#12754=CARTESIAN_POINT('Ctrl Pts',(95.9461441151234,0.692927346047603,2.09413232587469));
#12755=CARTESIAN_POINT('Ctrl Pts',(95.9412934059743,0.776232806747002,2.06278419368815));
#12756=CARTESIAN_POINT('Ctrl Pts',(95.9372203410383,0.846183104841956,2.03646165525239));
#12757=CARTESIAN_POINT('Ctrl Pts',(95.9331472761023,0.914927859152941,2.00652623511549));
#12758=CARTESIAN_POINT('Ctrl Pts',(95.9290742111664,0.982067987979568,1.97310883303121));
#12759=CARTESIAN_POINT('Ctrl Pts',(95.9250071303613,1.04910947479376,1.93974052766225));
#12760=CARTESIAN_POINT('Ctrl Pts',(95.9209400495562,1.11455059284824,1.90290060810877));
#12761=CARTESIAN_POINT('Ctrl Pts',(95.9168729687512,1.17801060799517,1.86276864034449));
#12762=CARTESIAN_POINT('Ctrl Pts',(95.9128106463823,1.2413963756789,1.82268362650533));
#12763=CARTESIAN_POINT('Ctrl Pts',(95.9087483240135,1.30280524401684,1.77931447073365));
#12764=CARTESIAN_POINT('Ctrl Pts',(95.9046860016446,1.36188101108845,1.73288664131175));
#12765=CARTESIAN_POINT('Ctrl Pts',(95.9006262575053,1.42091928460951,1.68648827818806));
#12766=CARTESIAN_POINT('Ctrl Pts',(95.896566513366,1.47762702079588,1.63703538788661));
#12767=CARTESIAN_POINT('Ctrl Pts',(95.8925067692267,1.53167807883756,1.58479596882643));
#12768=CARTESIAN_POINT('Ctrl Pts',(95.8884482897716,1.58571229899001,1.53257282329692));
#12769=CARTESIAN_POINT('Ctrl Pts',(95.8843898103166,1.63709114107314,1.47756520409031));
#12770=CARTESIAN_POINT('Ctrl Pts',(95.8803313308615,1.68552378756024,1.42007942086652));
#12771=CARTESIAN_POINT('Ctrl Pts',(95.8762728042292,1.73395699704716,1.36259296940574));
#12772=CARTESIAN_POINT('Ctrl Pts',(95.8722142775968,1.77944363667206,1.30262866302669));
#12773=CARTESIAN_POINT('Ctrl Pts',(95.8681557509644,1.82173286828323,1.24052624180892));
#12774=CARTESIAN_POINT('Ctrl Pts',(95.8640930739793,1.86406534593982,1.17836031307337));
#12775=CARTESIAN_POINT('Ctrl Pts',(95.8600303969942,1.90319361674,1.11405229872748));
#12776=CARTESIAN_POINT('Ctrl Pts',(95.8559677200091,1.93891037713846,1.04797068156739));
#12777=CARTESIAN_POINT('Ctrl Pts',(95.8519029210321,1.97464579289105,0.98185454907175));
#12778=CARTESIAN_POINT('Ctrl Pts',(95.847838122055,2.00696594438313,0.913963400475804));
#12779=CARTESIAN_POINT('Ctrl Pts',(95.843773323078,2.03571087317361,0.844687658748921));
#12780=CARTESIAN_POINT('Ctrl Pts',(95.839701262836,2.06450715125482,0.77528816440368));
#12781=CARTESIAN_POINT('Ctrl Pts',(95.835629202594,2.08971528929234,0.704499586951367));
#12782=CARTESIAN_POINT('Ctrl Pts',(95.831557142352,2.11122473453427,0.632729104981504));
#12783=CARTESIAN_POINT('Ctrl Pts',(95.8284189915531,2.12780108133615,0.577418873318676));
#12784=CARTESIAN_POINT('Ctrl Pts',(95.8252808407542,2.14218175830437,0.521525839307777));
#12785=CARTESIAN_POINT('Ctrl Pts',(95.8221426899553,2.1543370382082,0.465239643414357));
#12786=CARTESIAN_POINT('Ctrl Pts',(95.8180696250193,2.17011360458,0.392184731281153));
#12787=CARTESIAN_POINT('Ctrl Pts',(95.8139965600833,2.18220037643508,0.318185538243844));
#12788=CARTESIAN_POINT('Ctrl Pts',(95.8099234951473,2.19049114360055,0.243648414334174));
#12789=CARTESIAN_POINT('Ctrl Pts',(95.8058564143422,2.19876973000362,0.169220800072788));
#12790=CARTESIAN_POINT('Ctrl Pts',(95.8017893335372,2.20326333214251,0.0942572946533874));
#12791=CARTESIAN_POINT('Ctrl Pts',(95.7977222527321,2.203916584601,0.0191751954530534));
#12792=CARTESIAN_POINT('Ctrl Pts',(95.7936599303632,2.20456907276188,-0.0558190585838011));
#12793=CARTESIAN_POINT('Ctrl Pts',(95.7895976079943,2.20139013399951,-0.130931155687019));
#12794=CARTESIAN_POINT('Ctrl Pts',(95.7855352856255,2.19437627558659,-0.205739546861371));
#12795=CARTESIAN_POINT('Ctrl Pts',(95.7814755414861,2.18736686865129,-0.280500459478317));
#12796=CARTESIAN_POINT('Ctrl Pts',(95.7774157973468,2.17652741634232,-0.354957574492192));
#12797=CARTESIAN_POINT('Ctrl Pts',(95.7733560532075,2.16190645999275,-0.428691565395923));
#12798=CARTESIAN_POINT('Ctrl Pts',(95.7692975737525,2.14729005833742,-0.502402586818363));
#12799=CARTESIAN_POINT('Ctrl Pts',(95.7652390942974,2.12889458433321,-0.575390463351062));
#12800=CARTESIAN_POINT('Ctrl Pts',(95.7611806148423,2.10681991856933,-0.647244799685204));
#12801=CARTESIAN_POINT('Ctrl Pts',(95.7571220882099,2.08474499620098,-0.71909997128198));
#12802=CARTESIAN_POINT('Ctrl Pts',(95.7530635615775,2.05899093908381,-0.789821120635661));
#12803=CARTESIAN_POINT('Ctrl Pts',(95.7490050349451,2.0297073875272,-0.859013341582951));
#12804=CARTESIAN_POINT('Ctrl Pts',(95.74494235796,2.0003938898649,-0.928276320257746));
#12805=CARTESIAN_POINT('Ctrl Pts',(95.7408796809749,1.9675438766001,-0.996006807583816));
#12806=CARTESIAN_POINT('Ctrl Pts',(95.7368170039898,1.93135473407245,-1.06183091458854));
#12807=CARTESIAN_POINT('Ctrl Pts',(95.7327522050128,1.89514668945899,-1.12768940242773));
#12808=CARTESIAN_POINT('Ctrl Pts',(95.7286874060357,1.85559629380616,-1.19163912059643));
#12809=CARTESIAN_POINT('Ctrl Pts',(95.7246226070587,1.81294502659153,-1.25333408577164));
#12810=CARTESIAN_POINT('Ctrl Pts',(95.7205505468166,1.77021756811771,-1.3151392614374));
#12811=CARTESIAN_POINT('Ctrl Pts',(95.7164784865746,1.72437846540206,-1.37468125991971));
#12812=CARTESIAN_POINT('Ctrl Pts',(95.7124064263326,1.6757100499405,-1.43164654455225));
#12813=CARTESIAN_POINT('Ctrl Pts',(95.7092682755337,1.63820352553184,-1.47554708699346));
#12814=CARTESIAN_POINT('Ctrl Pts',(95.7061301247349,1.59901750013507,-1.51791795593156));
#12815=CARTESIAN_POINT('Ctrl Pts',(95.702991973936,1.55829525863933,-1.558631414704));
#12816=CARTESIAN_POINT('Ctrl Pts',(95.698918909,1.50544109560459,-1.611474178477));
#12817=CARTESIAN_POINT('Ctrl Pts',(95.694845844064,1.44979406352332,-1.66172732210596));
#12818=CARTESIAN_POINT('Ctrl Pts',(95.690772779128,1.3916381503919,-1.7090814077667));
#12819=CARTESIAN_POINT('Ctrl Pts',(95.686705698323,1.33356767969855,-1.75636592099167));
#12820=CARTESIAN_POINT('Ctrl Pts',(95.6826386175179,1.27299601341587,-1.80075953369305));
#12821=CARTESIAN_POINT('Ctrl Pts',(95.6785715367128,1.21024388945352,-1.84198961127375));
#12822=CARTESIAN_POINT('Ctrl Pts',(95.674509214344,1.14756518473018,-1.88317145015384));
#12823=CARTESIAN_POINT('Ctrl Pts',(95.6704468919751,1.08271148783142,-1.92119684668641));
#12824=CARTESIAN_POINT('Ctrl Pts',(95.6663845696062,1.01603521581505,-1.95583446135497));
#12825=CARTESIAN_POINT('Ctrl Pts',(95.6623248254669,0.949401261153161,-1.99045009260762));
#12826=CARTESIAN_POINT('Ctrl Pts',(95.6582650813276,0.88094744940858,-2.0216819891268));
#12827=CARTESIAN_POINT('Ctrl Pts',(95.6542053371883,0.811052522772792,-2.04934374991213));
#12828=CARTESIAN_POINT('Ctrl Pts',(95.6501468577333,0.741179369679854,-2.07699689355508));
#12829=CARTESIAN_POINT('Ctrl Pts',(95.6460883782783,0.669866436701337,-2.1010819340282));
#12830=CARTESIAN_POINT('Ctrl Pts',(95.6420298988232,0.597512776071211,-2.12146045978512));
#12831=CARTESIAN_POINT('Ctrl Pts',(95.6379713721908,0.525158274374103,-2.14183922242992));
#12832=CARTESIAN_POINT('Ctrl Pts',(95.6339128455584,0.451763481070672,-2.15851125709418));
#12833=CARTESIAN_POINT('Ctrl Pts',(95.6298543189261,0.377741390695677,-2.17138836732522));
#12834=CARTESIAN_POINT('Ctrl Pts',(95.625791641941,0.303643603445691,-2.18427864601717));
#12835=CARTESIAN_POINT('Ctrl Pts',(95.6217289649559,0.228917709546249,-2.1933661685537));
#12836=CARTESIAN_POINT('Ctrl Pts',(95.6176662879708,0.153984908484414,-2.19861425628941));
#12837=CARTESIAN_POINT('Ctrl Pts',(95.6136014889937,0.0790129689921754,
-2.20386508517337));
#12838=CARTESIAN_POINT('Ctrl Pts',(95.6095366900167,0.003834384947001,-2.20527247677358));
#12839=CARTESIAN_POINT('Ctrl Pts',(95.6054718910397,-0.071129208133638,
-2.20285193232552));
#12840=CARTESIAN_POINT('Ctrl Pts',(95.6013998307977,-0.146226714481638,
-2.20042706387161));
#12841=CARTESIAN_POINT('Ctrl Pts',(95.5973277705557,-0.221107986241424,
-2.19416064059518));
#12842=CARTESIAN_POINT('Ctrl Pts',(95.5932557103136,-0.295356524660395,
-2.18412007988126));
#12843=CARTESIAN_POINT('Ctrl Pts',(95.5901175595148,-0.352576481219793,
-2.17638227843606));
#12844=CARTESIAN_POINT('Ctrl Pts',(95.5869794087159,-0.409420744171687,
-2.16640405763089));
#12845=CARTESIAN_POINT('Ctrl Pts',(95.583841257917,-0.465704316896587,-2.15423663723925));
#12846=CARTESIAN_POINT('Ctrl Pts',(95.579768192981,-0.538755824370337,-2.13844431349996));
#12847=CARTESIAN_POINT('Ctrl Pts',(95.575695128045,-0.611144004893231,-2.11890149014625));
#12848=CARTESIAN_POINT('Ctrl Pts',(95.571622063109,-0.682454907239795,-2.09567919767896));
#12849=CARTESIAN_POINT('Ctrl Pts',(95.567554982304,-0.753661039890029,-2.07249102331213));
#12850=CARTESIAN_POINT('Ctrl Pts',(95.5634879014989,-0.823792586508467,
-2.04563425928801));
#12851=CARTESIAN_POINT('Ctrl Pts',(95.5594208206938,-0.892446616911418,
-2.01523076494067));
#12852=CARTESIAN_POINT('Ctrl Pts',(95.555358498325,-0.96102032291499,-1.98486284232027));
#12853=CARTESIAN_POINT('Ctrl Pts',(95.5512961759561,-1.02811951281543,-1.95095662611143));
#12854=CARTESIAN_POINT('Ctrl Pts',(95.5472338535872,-1.09335880029237,-1.91368297631118));
#12855=CARTESIAN_POINT('Ctrl Pts',(95.5431741094479,-1.15855668242417,-1.8764329829363));
#12856=CARTESIAN_POINT('Ctrl Pts',(95.5391143653086,-1.22189659103513,-1.83582003328102));
#12857=CARTESIAN_POINT('Ctrl Pts',(95.5350546211693,-1.28301664686955,-1.79206146207534));
#12858=CARTESIAN_POINT('Ctrl Pts',(95.5309961417142,-1.34411766269323,-1.7483165224617));
#12859=CARTESIAN_POINT('Ctrl Pts',(95.5269376622592,-1.4029998107652,-1.70142818464707));
#12860=CARTESIAN_POINT('Ctrl Pts',(95.5228791828041,-1.45933054229003,-1.65165685550586));
#12861=CARTESIAN_POINT('Ctrl Pts',(95.5188206561717,-1.51566192862509,-1.60188494780344));
#12862=CARTESIAN_POINT('Ctrl Pts',(95.5147621295393,-1.56944148290727,-1.54923029971699));
#12863=CARTESIAN_POINT('Ctrl Pts',(95.5107036029069,-1.62037130761176,-1.49399224411259));
#12864=CARTESIAN_POINT('Ctrl Pts',(95.5066409259218,-1.6713532144522,-1.43869770066557));
#12865=CARTESIAN_POINT('Ctrl Pts',(95.5025782489367,-1.71947924784372,-1.3808148258672));
#12866=CARTESIAN_POINT('Ctrl Pts',(95.4985155719516,-1.76449036506856,-1.32067776220403));
#12867=CARTESIAN_POINT('Ctrl Pts',(95.4944507729746,-1.80952499221767,-1.26050928812716));
#12868=CARTESIAN_POINT('Ctrl Pts',(95.4903859739975,-1.85144119684918,-1.1980846772798));
#12869=CARTESIAN_POINT('Ctrl Pts',(95.4863211750204,-1.89002355688284,-1.13376671076018));
#12870=CARTESIAN_POINT('Ctrl Pts',(95.4822491147784,-1.92867483957191,-1.06933384807972));
#12871=CARTESIAN_POINT('Ctrl Pts',(95.4781770545364,-1.96398015734139,-1.00300129605404));
#12872=CARTESIAN_POINT('Ctrl Pts',(95.4741049942944,-1.99577050653869,-0.935155647595793));
#12873=CARTESIAN_POINT('Ctrl Pts',(95.4709668434955,-2.02026987634191,-0.882870105816989));
#12874=CARTESIAN_POINT('Ctrl Pts',(95.4678286926966,-2.04268262813904,-0.82968642713777));
#12875=CARTESIAN_POINT('Ctrl Pts',(95.4646905418978,-2.06295157688694,-0.7757878520702));
#12876=CARTESIAN_POINT('Ctrl Pts',(95.4606174769618,-2.08925902663219,-0.705831877906623));
#12877=CARTESIAN_POINT('Ctrl Pts',(95.4565444120258,-2.11205479901269,-0.634401328520342));
#12878=CARTESIAN_POINT('Ctrl Pts',(95.4524713470898,-2.13117430748127,-0.561882613302562));
#12879=CARTESIAN_POINT('Ctrl Pts',(95.4484042662847,-2.15026572564346,-0.489470442295007));
#12880=CARTESIAN_POINT('Ctrl Pts',(95.4443371854797,-2.1656914826729,-0.415973737436818));
#12881=CARTESIAN_POINT('Ctrl Pts',(95.4402701046746,-2.17733568478907,-0.341797185102692));
#12882=CARTESIAN_POINT('Ctrl Pts',(95.4362077823057,-2.18896626332719,-0.267707418452967));
#12883=CARTESIAN_POINT('Ctrl Pts',(95.4321454599369,-2.19682400350121,-0.192939853946335));
#12884=CARTESIAN_POINT('Ctrl Pts',(95.428083137568,-2.20084370192936,-0.117910982007089));
#12885=CARTESIAN_POINT('Ctrl Pts',(95.4240233934287,-2.20486084918003,-0.0429297285575062));
#12886=CARTESIAN_POINT('Ctrl Pts',(95.4199636492894,-2.20504476295785,0.032312027657186));
#12887=CARTESIAN_POINT('Ctrl Pts',(95.4159039051501,-2.20138203823516,0.107392372800067));
#12888=CARTESIAN_POINT('Ctrl Pts',(95.411845425695,-2.19772045451793,0.182449329047782));
#12889=CARTESIAN_POINT('Ctrl Pts',(95.40778694624,-2.19021463471915,0.257344497474993));
#12890=CARTESIAN_POINT('Ctrl Pts',(95.4037284667849,-2.17890326754456,0.331657278954689));
#12891=CARTESIAN_POINT('Ctrl Pts',(95.3996699401525,-2.16759176888227,0.405970924274905));
#12892=CARTESIAN_POINT('Ctrl Pts',(95.3956114135202,-2.15247470863038,0.479701697451623));
#12893=CARTESIAN_POINT('Ctrl Pts',(95.3915528868878,-2.13364226733496,0.552437032648741));
#12894=CARTESIAN_POINT('Ctrl Pts',(95.3874902099027,-2.11479056750539,0.625246748852262));
#12895=CARTESIAN_POINT('Ctrl Pts',(95.3834275329176,-2.09221601930329,0.697058531022004));
#12896=CARTESIAN_POINT('Ctrl Pts',(95.3793648559325,-2.06605911289123,0.767473609995231));
#12897=CARTESIAN_POINT('Ctrl Pts',(95.3753000569555,-2.03988854436796,0.837925467730612));
#12898=CARTESIAN_POINT('Ctrl Pts',(95.3712352579784,-2.01013208061837,0.906978730617126));
#12899=CARTESIAN_POINT('Ctrl Pts',(95.3671704590014,-1.97697791694915,0.974255775397501));
#12900=CARTESIAN_POINT('Ctrl Pts',(95.3630983987593,-1.94376452743175,1.04165300236919));
#12901=CARTESIAN_POINT('Ctrl Pts',(95.3590263385173,-1.90714154754015,1.10726725588856));
#12902=CARTESIAN_POINT('Ctrl Pts',(95.3549542782753,-1.8673423367302,1.17074702538806));
#12903=CARTESIAN_POINT('Ctrl Pts',(95.3518161274765,-1.83667090316217,1.21966798370595));
#12904=CARTESIAN_POINT('Ctrl Pts',(95.3486779766776,-1.8041140182598,1.26732178068403));
#12905=CARTESIAN_POINT('Ctrl Pts',(95.3455398258787,-1.76979471058198,1.31356106915363));
#12906=CARTESIAN_POINT('Ctrl Pts',(95.3415053544189,-1.72567310004701,1.37300725310416));
#12907=CARTESIAN_POINT('Ctrl Pts',(95.337470882959,-1.67845985876083,1.43035320436202));
#12908=CARTESIAN_POINT('Ctrl Pts',(95.3334364114992,-1.62838390961034,1.48525480740584));
#12909=CARTESIAN_POINT('Ctrl Pts',(95.3293038463307,-1.57709041917589,1.54149128216742));
#12910=CARTESIAN_POINT('Ctrl Pts',(95.3251712811623,-1.52279341517083,1.59516252052928));
#12911=CARTESIAN_POINT('Ctrl Pts',(95.3210387159939,-1.4657859356181,1.64593061547082));
#12912=CARTESIAN_POINT('Ctrl Pts',(95.3170149216926,-1.41027891709368,1.69536247263202));
#12913=CARTESIAN_POINT('Ctrl Pts',(95.3129911273913,-1.35220273106132,1.74204177364241));
#12914=CARTESIAN_POINT('Ctrl Pts',(95.30896733309,-1.29186683262772,1.78569204701047));
#12915=CARTESIAN_POINT('Ctrl Pts',(95.3049459527131,-1.23156713045278,1.82931613403462));
#12916=CARTESIAN_POINT('Ctrl Pts',(95.3009245723363,-1.16901079881204,1.86991451268246));
#12917=CARTESIAN_POINT('Ctrl Pts',(95.2969031919594,-1.10453991000684,1.90725131726316));
#12918=CARTESIAN_POINT('Ctrl Pts',(95.292882863597,-1.04008588712866,1.94457835433744));
#12919=CARTESIAN_POINT('Ctrl Pts',(95.2888625352346,-0.973718723115101,
1.97864526717714));
#12920=CARTESIAN_POINT('Ctrl Pts',(95.2848422068722,-0.905807482380869,
2.00926076079309));
#12921=CARTESIAN_POINT('Ctrl Pts',(95.2806265935876,-0.834597495831594,
2.04136338275995));
#12922=CARTESIAN_POINT('Ctrl Pts',(95.2764109803031,-0.761690125013591,
2.06967047871341));
#12923=CARTESIAN_POINT('Ctrl Pts',(95.2721953670185,-0.687535305187299,
2.09401795697196));
#12924=CARTESIAN_POINT('Ctrl Pts',(95.268170641133,-0.616738293520773,2.11726295583189));
#12925=CARTESIAN_POINT('Ctrl Pts',(95.2641459152475,-0.5448048662267,2.13689908807007));
#12926=CARTESIAN_POINT('Ctrl Pts',(95.260121189362,-0.472140595541541,2.15283516741103));
#12927=CARTESIAN_POINT('Ctrl Pts',(95.2560939465934,-0.399430883880333,
2.16878121246132));
#12928=CARTESIAN_POINT('Ctrl Pts',(95.2520667038249,-0.325989900197102,
2.18102252395255));
#12929=CARTESIAN_POINT('Ctrl Pts',(95.2480394610563,-0.252230387745128,
2.18951954352957));
#12930=CARTESIAN_POINT('Ctrl Pts',(95.2440061136435,-0.178359067883193,
2.19802944320463));
#12931=CARTESIAN_POINT('Ctrl Pts',(95.2399727662307,-0.1041687412949,2.20278370595594));
#12932=CARTESIAN_POINT('Ctrl Pts',(95.2359394188179,-0.0300731305126705,
2.20379481958307));
#12933=CARTESIAN_POINT('Ctrl Pts',(95.235377895031,-0.0197575182690645,
2.20393558711304));
#12934=CARTESIAN_POINT('Ctrl Pts',(95.2348163712442,-0.00944373356853099,
2.20400388601063));
#12935=CARTESIAN_POINT('Ctrl Pts',(95.2342548474574,0.000867116891639564,
2.20399982942565));
#12936=CARTESIAN_POINT('',(94.484254847381,-0.00201577163552605,2.20399907819053));
#12937=CARTESIAN_POINT('Ctrl Pts',(95.23425484741,0.000867117761720935,
2.20399982942531));
#12938=CARTESIAN_POINT('Ctrl Pts',(95.2316329348932,0.0490113789919599,
2.20398088806992));
#12939=CARTESIAN_POINT('Ctrl Pts',(95.2290110223763,0.0971228006821106,
2.20238457773465));
#12940=CARTESIAN_POINT('Ctrl Pts',(95.2263891098594,0.145129365900741,2.19921655758437));
#12941=CARTESIAN_POINT('Ctrl Pts',(95.2223160449234,0.219706170516748,2.19429513030269));
#12942=CARTESIAN_POINT('Ctrl Pts',(95.2182429799874,0.294176174713683,2.18556649358735));
#12943=CARTESIAN_POINT('Ctrl Pts',(95.2141699150513,0.368119487752487,2.17304027637245));
#12944=CARTESIAN_POINT('Ctrl Pts',(95.2101028342462,0.441954163567666,2.16053246262643));
#12945=CARTESIAN_POINT('Ctrl Pts',(95.2060357534412,0.515263217712541,2.14423822483221));
#12946=CARTESIAN_POINT('Ctrl Pts',(95.2019686726361,0.587630216226328,2.1242190868594));
#12947=CARTESIAN_POINT('Ctrl Pts',(95.1979063502672,0.659912546212096,2.10422337104005));
#12948=CARTESIAN_POINT('Ctrl Pts',(95.1938440278984,0.731254552509463,2.08051154023093));
#12949=CARTESIAN_POINT('Ctrl Pts',(95.1897817055295,0.801249978189934,2.05319616024642));
#12950=CARTESIAN_POINT('Ctrl Pts',(95.1857219613902,0.8712009799524,2.02589811648336));
#12951=CARTESIAN_POINT('Ctrl Pts',(95.1816622172509,0.939806653360161,1.99500123510716));
#12952=CARTESIAN_POINT('Ctrl Pts',(95.1776024731116,1.00667718739468,1.96066749867976));
#12953=CARTESIAN_POINT('Ctrl Pts',(95.1735439936566,1.07352689003975,1.92634445783667));
#12954=CARTESIAN_POINT('Ctrl Pts',(95.1694855142016,1.13864210203628,1.88858690559608));
#12955=CARTESIAN_POINT('Ctrl Pts',(95.1654270347466,1.20165571726809,1.847603728389));
#12956=CARTESIAN_POINT('Ctrl Pts',(95.1613685081143,1.26467006499454,1.8066200747776));
#12957=CARTESIAN_POINT('Ctrl Pts',(95.1573099814819,1.32558236817435,1.7624109835724));
#12958=CARTESIAN_POINT('Ctrl Pts',(95.1532514548496,1.38405409633897,1.71522892303252));
#12959=CARTESIAN_POINT('Ctrl Pts',(95.1491887778645,1.44258561918211,1.6679986129158));
#12960=CARTESIAN_POINT('Ctrl Pts',(95.1451261008795,1.49867121064966,1.61778956278921));
#12961=CARTESIAN_POINT('Ctrl Pts',(95.1410634238944,1.55200567708095,1.56489436650162));
#12962=CARTESIAN_POINT('Ctrl Pts',(95.1369986249174,1.60536800083603,1.51197154232707));
#12963=CARTESIAN_POINT('Ctrl Pts',(95.1329338259405,1.65597601635295,1.45636013148767));
#12964=CARTESIAN_POINT('Ctrl Pts',(95.1288690269635,1.70356348513045,1.39838744707259));
#12965=CARTESIAN_POINT('Ctrl Pts',(95.1247969667215,1.751235963086,1.34031120156511));
#12966=CARTESIAN_POINT('Ctrl Pts',(95.1207249064795,1.79587683246783,1.27986564174607));
#12967=CARTESIAN_POINT('Ctrl Pts',(95.1166528462376,1.83726228457379,1.21740843503021));
#12968=CARTESIAN_POINT('Ctrl Pts',(95.1135146954386,1.86915616184366,1.16927551913227));
#12969=CARTESIAN_POINT('Ctrl Pts',(95.1103765446396,1.89911748674715,1.11994850694536));
#12970=CARTESIAN_POINT('Ctrl Pts',(95.1072383938406,1.92706285005977,1.0696002860506));
#12971=CARTESIAN_POINT('Ctrl Pts',(95.1031653289046,1.96333366262495,1.00425238333646));
#12972=CARTESIAN_POINT('Ctrl Pts',(95.0990922639686,1.99634667105031,0.936931421528423));
#12973=CARTESIAN_POINT('Ctrl Pts',(95.0950191990326,2.02588246297701,0.867995533515123));
#12974=CARTESIAN_POINT('Ctrl Pts',(95.0909521182276,2.05537486103475,0.7991609258365));
#12975=CARTESIAN_POINT('Ctrl Pts',(95.0868850374225,2.08139999899706,0.728716537848663));
#12976=CARTESIAN_POINT('Ctrl Pts',(95.0828179566175,2.10378395485132,0.657045714779518));
#12977=CARTESIAN_POINT('Ctrl Pts',(95.0787556342486,2.12614172174337,0.585458745721258));
#12978=CARTESIAN_POINT('Ctrl Pts',(95.0746933118797,2.14486662882977,0.512648645889528));
#12979=CARTESIAN_POINT('Ctrl Pts',(95.0706309895108,2.1598331686819,0.439017862349023));
#12980=CARTESIAN_POINT('Ctrl Pts',(95.0665712453715,2.17479020973704,0.365433809974987));
#12981=CARTESIAN_POINT('Ctrl Pts',(95.0625115012322,2.18599352210005,0.291030574194199));
#12982=CARTESIAN_POINT('Ctrl Pts',(95.0584517570929,2.19336804356406,0.216223554387558));
#12983=CARTESIAN_POINT('Ctrl Pts',(95.0543932776378,2.20074026773029,0.141439838330293));
#12984=CARTESIAN_POINT('Ctrl Pts',(95.0503347981827,2.20428602231726,0.0662530628375085));
#12985=CARTESIAN_POINT('Ctrl Pts',(95.0462763187276,2.2039819695306,-0.00891504256971563));
#12986=CARTESIAN_POINT('Ctrl Pts',(95.0422177920952,2.20367791320951,-0.0840840217600974));
#12987=CARTESIAN_POINT('Ctrl Pts',(95.0381592654628,2.199523964383,-0.159233852984441));
#12988=CARTESIAN_POINT('Ctrl Pts',(95.0341007388304,2.19154889840338,-0.233943210858857));
#12989=CARTESIAN_POINT('Ctrl Pts',(95.0300380618453,2.18356567691815,-0.308728968425563));
#12990=CARTESIAN_POINT('Ctrl Pts',(95.0259753848602,2.17175358587468,-0.383072877322738));
#12991=CARTESIAN_POINT('Ctrl Pts',(95.021912707875,2.15619318851793,-0.456559890692193));
#12992=CARTESIAN_POINT('Ctrl Pts',(95.017847908898,2.14062466375209,-0.530085287337291));
#12993=CARTESIAN_POINT('Ctrl Pts',(95.0137831099209,2.12130405671947,-0.602752435307004));
#12994=CARTESIAN_POINT('Ctrl Pts',(95.0097183109438,2.09836221869048,-0.674160217731919));
#12995=CARTESIAN_POINT('Ctrl Pts',(95.0056462507018,2.07537939788088,-0.745695561404457));
#12996=CARTESIAN_POINT('Ctrl Pts',(95.0015741904597,2.04876259435406,-0.815966598760288));
#12997=CARTESIAN_POINT('Ctrl Pts',(94.9975021302177,2.01869116135146,-0.884591428333714));
#12998=CARTESIAN_POINT('Ctrl Pts',(94.9943639794188,1.99551648173194,-0.937477449401332));
#12999=CARTESIAN_POINT('Ctrl Pts',(94.99122582862,1.97029107455252,-0.989386157279503));
#13000=CARTESIAN_POINT('Ctrl Pts',(94.9880876778211,1.94311505799379,-1.04015377295754));
#13001=CARTESIAN_POINT('Ctrl Pts',(94.9840146128851,1.90784279504664,-1.10604601605083));
#13002=CARTESIAN_POINT('Ctrl Pts',(94.9799415479491,1.86914704219674,-1.1702691375526));
#13003=CARTESIAN_POINT('Ctrl Pts',(94.9758684830131,1.82720992594269,-1.23244467889496));
#13004=CARTESIAN_POINT('Ctrl Pts',(94.971801402208,1.78533442353437,-1.29452887217732));
#13005=CARTESIAN_POINT('Ctrl Pts',(94.967734321403,1.74022727740138,-1.35457106544739));
#13006=CARTESIAN_POINT('Ctrl Pts',(94.9636672405979,1.69211645247092,-1.41221737394681));
#13007=CARTESIAN_POINT('Ctrl Pts',(94.9596049182291,1.64406191663366,-1.46979623695062));
#13008=CARTESIAN_POINT('Ctrl Pts',(94.9555425958602,1.59301098844483,-1.52498441968892));
#13009=CARTESIAN_POINT('Ctrl Pts',(94.9514802734913,1.53923391983028,-1.57745837981352));
#13010=CARTESIAN_POINT('Ctrl Pts',(94.947420529352,1.48549098184732,-1.62989903634894));
#13011=CARTESIAN_POINT('Ctrl Pts',(94.9433607852127,1.42902567769116,-1.67962855604401));
#13012=CARTESIAN_POINT('Ctrl Pts',(94.9393010410734,1.37014647789114,-1.72635877763647));
#13013=CARTESIAN_POINT('Ctrl Pts',(94.9352425616184,1.31128562003442,-1.77307444191366));
#13014=CARTESIAN_POINT('Ctrl Pts',(94.9311840821634,1.2500127332865,-1.81679236654611));
#13015=CARTESIAN_POINT('Ctrl Pts',(94.9271256027083,1.18666963397142,-1.85726443454079));
#13016=CARTESIAN_POINT('Ctrl Pts',(94.9230670760759,1.1233257983316,-1.89773697299848));
#13017=CARTESIAN_POINT('Ctrl Pts',(94.9190085494436,1.05791210565424,-1.93496332434018));
#13018=CARTESIAN_POINT('Ctrl Pts',(94.9149500228112,0.990798268561067,-1.96873939134066));
#13019=CARTESIAN_POINT('Ctrl Pts',(94.9108873458261,0.923615799148664,-2.00254999860755));
#13020=CARTESIAN_POINT('Ctrl Pts',(94.906824668841,0.854730140856377,-2.03290306050522));
#13021=CARTESIAN_POINT('Ctrl Pts',(94.9027619918559,0.784533788984808,-2.05964140906643));
#13022=CARTESIAN_POINT('Ctrl Pts',(94.8986971928789,0.714300772595258,-2.08639372343405));
#13023=CARTESIAN_POINT('Ctrl Pts',(94.8946323939019,0.642756154050088,-2.10952741763499));
#13024=CARTESIAN_POINT('Ctrl Pts',(94.8905675949248,0.570307967659544,-2.12893513805002));
#13025=CARTESIAN_POINT('Ctrl Pts',(94.8864955346828,0.497730361467263,-2.14837752797789));
#13026=CARTESIAN_POINT('Ctrl Pts',(94.8824234744408,0.424246430975652,-2.16408054936068));
#13027=CARTESIAN_POINT('Ctrl Pts',(94.8783514141988,0.350274339422994,-2.17598802550515));
#13028=CARTESIAN_POINT('Ctrl Pts',(94.8752132634,0.293267427834428,-2.18516457338371));
#13029=CARTESIAN_POINT('Ctrl Pts',(94.8720751126011,0.235970816031289,-2.19208796827572));
#13030=CARTESIAN_POINT('Ctrl Pts',(94.8689369618022,0.178576405409072,-2.19675362010199));
#13031=CARTESIAN_POINT('Ctrl Pts',(94.8648638968662,0.10408312053836,-2.20280925734669));
#13032=CARTESIAN_POINT('Ctrl Pts',(94.8607908319302,0.0291378055903611,
-2.20508310681169));
#13033=CARTESIAN_POINT('Ctrl Pts',(94.8567177669943,-0.0458427673246245,
-2.20352318814303));
#13034=CARTESIAN_POINT('Ctrl Pts',(94.8526506861892,-0.120713179077782,
-2.20196556130072));
#13035=CARTESIAN_POINT('Ctrl Pts',(94.8485836053841,-0.195618272557399,
-2.19658535909733));
#13036=CARTESIAN_POINT('Ctrl Pts',(94.8445165245791,-0.270137093596187,
-2.18738244270713));
#13037=CARTESIAN_POINT('Ctrl Pts',(94.8404542022102,-0.344568728500258,
-2.1781902936197));
#13038=CARTESIAN_POINT('Ctrl Pts',(94.8363918798413,-0.41861451737398,-2.16518437446876));
#13039=CARTESIAN_POINT('Ctrl Pts',(94.8323295574724,-0.491856096706097,
-2.14841652854679));
#13040=CARTESIAN_POINT('Ctrl Pts',(94.8282698133331,-0.565051191887526,
-2.13165932465471));
#13041=CARTESIAN_POINT('Ctrl Pts',(94.8242100691938,-0.637442626134506,
-2.11114503816434));
#13042=CARTESIAN_POINT('Ctrl Pts',(94.8201503250545,-0.708621065909673,
-2.08697680508171));
#13043=CARTESIAN_POINT('Ctrl Pts',(94.8160918455994,-0.779777332304277,
-2.06281610084392));
#13044=CARTESIAN_POINT('Ctrl Pts',(94.8120333661444,-0.849720902656972,
-2.03500386341315));
#13045=CARTESIAN_POINT('Ctrl Pts',(94.8079748866893,-0.918058032970696,
-2.00369295254986));
#13046=CARTESIAN_POINT('Ctrl Pts',(94.8039163600569,-0.986395957661693,
-1.97238167771642));
#13047=CARTESIAN_POINT('Ctrl Pts',(94.7998578334245,-1.05312697191543,-1.93757184921118));
#13048=CARTESIAN_POINT('Ctrl Pts',(94.7957993067921,-1.11787921530799,-1.89946362428513));
#13049=CARTESIAN_POINT('Ctrl Pts',(94.791736629807,-1.18269767599392,-1.86131642891763));
#13050=CARTESIAN_POINT('Ctrl Pts',(94.7876739528219,-1.24553291251983,-1.81986434410088));
#13051=CARTESIAN_POINT('Ctrl Pts',(94.7836112758368,-1.30604016410821,-1.77535210303089));
#13052=CARTESIAN_POINT('Ctrl Pts',(94.7795464768597,-1.36657901946451,-1.73081661260649));
#13053=CARTESIAN_POINT('Ctrl Pts',(94.7754816778827,-1.42478709850043,-1.68321808547488));
#13054=CARTESIAN_POINT('Ctrl Pts',(94.7714168789056,-1.4803530897551,-1.63284130571606));
#13055=CARTESIAN_POINT('Ctrl Pts',(94.7673448186636,-1.53601834283991,-1.58237453401717));
#13056=CARTESIAN_POINT('Ctrl Pts',(94.7632727584216,-1.5890317434293,-1.52911993535198));
#13057=CARTESIAN_POINT('Ctrl Pts',(94.7592006981796,-1.63911950591113,-1.47339853581495));
#13058=CARTESIAN_POINT('Ctrl Pts',(94.7560625473807,-1.67771985622653,-1.43045659879045));
#13059=CARTESIAN_POINT('Ctrl Pts',(94.7529243965818,-1.71458341002876,-1.38605036587126));
#13060=CARTESIAN_POINT('Ctrl Pts',(94.7497862457829,-1.74960233326733,-1.34033864206981));
#13061=CARTESIAN_POINT('Ctrl Pts',(94.7457131808469,-1.79505405228274,-1.28100853612167));
#13062=CARTESIAN_POINT('Ctrl Pts',(94.7416401159109,-1.83757211974619,-1.21924945125779));
#13063=CARTESIAN_POINT('Ctrl Pts',(94.7375670509749,-1.8768870307861,-1.15538351800038));
#13064=CARTESIAN_POINT('Ctrl Pts',(94.7334999701698,-1.91614418051386,-1.09161141632008));
#13065=CARTESIAN_POINT('Ctrl Pts',(94.7294328893648,-1.95220726905968,-1.02573901504703));
#13066=CARTESIAN_POINT('Ctrl Pts',(94.7253658085597,-1.98484809813193,-0.958120048502315));
#13067=CARTESIAN_POINT('Ctrl Pts',(94.7213034861908,-2.01745073782221,-0.890580195344562));
#13068=CARTESIAN_POINT('Ctrl Pts',(94.717241163822,-2.04663886656072,-0.821298264629233));
#13069=CARTESIAN_POINT('Ctrl Pts',(94.7131788414531,-2.07222938039574,-0.750653978224795));
#13070=CARTESIAN_POINT('Ctrl Pts',(94.7091190973138,-2.09780365272815,-0.680054527550057));
#13071=CARTESIAN_POINT('Ctrl Pts',(94.7050593531745,-2.11978467890283,-0.608094884757306));
#13072=CARTESIAN_POINT('Ctrl Pts',(94.7009996090352,-2.13803735882198,-0.535174973519425));
#13073=CARTESIAN_POINT('Ctrl Pts',(94.6969411295802,-2.15628435269885,-0.462277778162198));
#13074=CARTESIAN_POINT('Ctrl Pts',(94.6928826501251,-2.17080519046376,-0.388421371160504));
#13075=CARTESIAN_POINT('Ctrl Pts',(94.6888241706701,-2.18151501127954,-0.314019514619797));
#13076=CARTESIAN_POINT('Ctrl Pts',(94.6847656440377,-2.19222495659042,-0.23961679320304));
#13077=CARTESIAN_POINT('Ctrl Pts',(94.6807071174053,-2.1991237307389,-0.164669082503113));
#13078=CARTESIAN_POINT('Ctrl Pts',(94.6766485907729,-2.20217808312383,-0.0895973783602944));
#13079=CARTESIAN_POINT('Ctrl Pts',(94.6725859137878,-2.20523555896731,-0.0144489039807578));
#13080=CARTESIAN_POINT('Ctrl Pts',(94.6685232368027,-2.20444074280571,0.0608233389258848));
#13081=CARTESIAN_POINT('Ctrl Pts',(94.6644605598176,-2.19981253300626,0.135796979453149));
#13082=CARTESIAN_POINT('Ctrl Pts',(94.6603957608406,-2.19518190582931,0.210809779741819));
#13083=CARTESIAN_POINT('Ctrl Pts',(94.6563309618636,-2.1867139515811,0.285523192199072));
#13084=CARTESIAN_POINT('Ctrl Pts',(94.6522661628865,-2.17447935469135,0.359521259484193));
#13085=CARTESIAN_POINT('Ctrl Pts',(94.6481941026445,-2.1622229021944,0.433651515243245));
#13086=CARTESIAN_POINT('Ctrl Pts',(94.6441220424025,-2.14618646915675,0.507063406217915));
#13087=CARTESIAN_POINT('Ctrl Pts',(94.6400499821605,-2.12649153348655,0.579352878658624));
#13088=CARTESIAN_POINT('Ctrl Pts',(94.6369118313616,-2.11131354631698,0.635063072566992));
#13089=CARTESIAN_POINT('Ctrl Pts',(94.6337736805628,-2.09396379492343,0.69010688463997));
#13090=CARTESIAN_POINT('Ctrl Pts',(94.6306355297639,-2.07451732729691,0.744307637166844));
#13091=CARTESIAN_POINT('Ctrl Pts',(94.6265624648279,-2.04927739126605,0.814655813137714));
#13092=CARTESIAN_POINT('Ctrl Pts',(94.6224893998919,-2.02040639988904,0.88385434260875));
#13093=CARTESIAN_POINT('Ctrl Pts',(94.618416334956,-1.98802907873226,0.951502171366401));
#13094=CARTESIAN_POINT('Ctrl Pts',(94.6143492541509,-1.95569932620795,1.019050612201));
#13095=CARTESIAN_POINT('Ctrl Pts',(94.6102821733458,-1.91987367612162,1.0850524485454));
#13096=CARTESIAN_POINT('Ctrl Pts',(94.6062150925408,-1.88072579760258,1.14912422054021));
#13097=CARTESIAN_POINT('Ctrl Pts',(94.6021527701719,-1.841623721636,1.21312102932351));
#13098=CARTESIAN_POINT('Ctrl Pts',(94.598090447803,-1.79920738744258,1.2751918548093));
#13099=CARTESIAN_POINT('Ctrl Pts',(94.5940281254341,-1.75369673957379,1.33497705808311));
#13100=CARTESIAN_POINT('Ctrl Pts',(94.5899683812948,-1.70821497589665,1.39472431754928));
#13101=CARTESIAN_POINT('Ctrl Pts',(94.5859086371555,-1.65964308408925,1.45218845444174));
#13102=CARTESIAN_POINT('Ctrl Pts',(94.5818488930162,-1.60824399767617,1.50703923105491));
#13103=CARTESIAN_POINT('Ctrl Pts',(94.5777904135612,-1.55686092301483,1.56187292065197));
#13104=CARTESIAN_POINT('Ctrl Pts',(94.5737319341061,-1.50265272864739,1.61409451817641));
#13105=CARTESIAN_POINT('Ctrl Pts',(94.569673454651,-1.44592119988364,1.66340851378339));
#13106=CARTESIAN_POINT('Ctrl Pts',(94.5656149280186,-1.38918901165063,1.71272308263534));
#13107=CARTESIAN_POINT('Ctrl Pts',(94.5615564013863,-1.32993379230777,1.7591296705784));
#13108=CARTESIAN_POINT('Ctrl Pts',(94.5574978747539,-1.26849137056239,1.80237222648618));
#13109=CARTESIAN_POINT('Ctrl Pts',(94.5534351977688,-1.20698611623151,1.84565900333308));
#13110=CARTESIAN_POINT('Ctrl Pts',(94.5493725207836,-1.1432895842801,1.88577501138828));
#13111=CARTESIAN_POINT('Ctrl Pts',(94.5453098437985,-1.07776701453231,1.9225072853922));
#13112=CARTESIAN_POINT('Ctrl Pts',(94.5412450448215,-1.01221022144705,1.95925874516699));
#13113=CARTESIAN_POINT('Ctrl Pts',(94.5371802458444,-0.94482591951831,1.99262273928844));
#13114=CARTESIAN_POINT('Ctrl Pts',(94.5331154468674,-0.876002016757105,
2.02243330338419));
#13115=CARTESIAN_POINT('Ctrl Pts',(94.5290433866254,-0.807055168532504,
2.05229712039745));
#13116=CARTESIAN_POINT('Ctrl Pts',(94.5249713263834,-0.73666403069448,2.07859466087012));
#13117=CARTESIAN_POINT('Ctrl Pts',(94.5208992661413,-0.665234027303954,
2.10120910166432));
#13118=CARTESIAN_POINT('Ctrl Pts',(94.5177611153424,-0.610186186927786,
2.11863701805723));
#13119=CARTESIAN_POINT('Ctrl Pts',(94.5146229645435,-0.55452173018533,2.13387851983892));
#13120=CARTESIAN_POINT('Ctrl Pts',(94.5114848137447,-0.49842981621141,2.14690095680063));
#13121=CARTESIAN_POINT('Ctrl Pts',(94.5060042023378,-0.400468308540214,
2.16964394180405));
#13122=CARTESIAN_POINT('Ctrl Pts',(94.5005235909309,-0.300897817452928,
2.18569009051323));
#13123=CARTESIAN_POINT('Ctrl Pts',(94.4950429795241,-0.200495865891814,
2.19486159193702));
#13124=CARTESIAN_POINT('Ctrl Pts',(94.4914469354861,-0.134618208726679,
2.2008793736344));
#13125=CARTESIAN_POINT('Ctrl Pts',(94.487850891448,-0.0683829464465262,
2.20393837893462));
#13126=CARTESIAN_POINT('Ctrl Pts',(94.48425484741,-0.00201577217147137,
2.20399907819004));
#13127=CARTESIAN_POINT('',(93.734254847381,0.000279264059390885,2.20399998230753));
#13128=CARTESIAN_POINT('Ctrl Pts',(94.484254847381,-0.00201577163552312,
2.20399907819053));
#13129=CARTESIAN_POINT('Ctrl Pts',(94.4802443723136,0.0719999787032919,
2.20406677279694));
#13130=CARTESIAN_POINT('Ctrl Pts',(94.4762338972462,0.146123122639629,2.20040178212574));
#13131=CARTESIAN_POINT('Ctrl Pts',(94.4722234221788,0.21994154036407,2.19299833990413));
#13132=CARTESIAN_POINT('Ctrl Pts',(94.4682158556641,0.293706422096562,2.18560026694721));
#13133=CARTESIAN_POINT('Ctrl Pts',(94.4642082891495,0.367166528766565,2.17446916659792));
#13134=CARTESIAN_POINT('Ctrl Pts',(94.4602007226348,0.439911613805786,2.15965130797515));
#13135=CARTESIAN_POINT('Ctrl Pts',(94.4561946870196,0.512628910058618,2.14483910980777));
#13136=CARTESIAN_POINT('Ctrl Pts',(94.4521886514044,0.584631245720701,2.1263430451521));
#13137=CARTESIAN_POINT('Ctrl Pts',(94.4481826157892,0.655517147150896,2.10426074187377));
#13138=CARTESIAN_POINT('Ctrl Pts',(94.4441767355832,0.726400298648532,2.08217929525161));
#13139=CARTESIAN_POINT('Ctrl Pts',(94.4401708553773,0.796166633606758,2.0565120343155));
#13140=CARTESIAN_POINT('Ctrl Pts',(94.4361649751714,0.864430195458748,2.02740633252911));
#13141=CARTESIAN_POINT('Ctrl Pts',(94.4321552226181,0.932759745360509,1.99827249525659));
#13142=CARTESIAN_POINT('Ctrl Pts',(94.4281454700648,0.999583169482648,1.96569377490942));
#13143=CARTESIAN_POINT('Ctrl Pts',(94.4241357175115,1.06453577329586,1.92986517336663));
#13144=CARTESIAN_POINT('Ctrl Pts',(94.4201239061042,1.12952172777926,1.89401817521148));
#13145=CARTESIAN_POINT('Ctrl Pts',(94.4161120946968,1.19263453356797,1.85491823532025));
#13146=CARTESIAN_POINT('Ctrl Pts',(94.4121002832894,1.25353773672876,1.81280422070254));
#13147=CARTESIAN_POINT('Ctrl Pts',(94.4080815480228,1.31454605081407,1.77061752283039));
#13148=CARTESIAN_POINT('Ctrl Pts',(94.4040628127562,1.37333676154219,1.72540666685662));
#13149=CARTESIAN_POINT('Ctrl Pts',(94.4000440774896,1.42960639689859,1.67745090835667));
#13150=CARTESIAN_POINT('Ctrl Pts',(94.3974740842349,1.46559099745434,1.64678305698287));
#13151=CARTESIAN_POINT('Ctrl Pts',(94.3949040909802,1.50054528958034,1.61499341728707));
#13152=CARTESIAN_POINT('Ctrl Pts',(94.3923340977256,1.53439831437836,1.58216238510238));
#13153=CARTESIAN_POINT('Ctrl Pts',(94.3882610327896,1.58805042729019,1.53012998160833));
#13154=CARTESIAN_POINT('Ctrl Pts',(94.3841879678536,1.63915632778103,1.47526507881002));
#13155=CARTESIAN_POINT('Ctrl Pts',(94.3801149029176,1.68740223239212,1.41784685566464));
#13156=CARTESIAN_POINT('Ctrl Pts',(94.3760478221125,1.73557725431059,1.36051299114606));
#13157=CARTESIAN_POINT('Ctrl Pts',(94.3719807413075,1.78090031822109,1.30063361671115));
#13158=CARTESIAN_POINT('Ctrl Pts',(94.3679136605024,1.82309387238746,1.23852522479896));
#13159=CARTESIAN_POINT('Ctrl Pts',(94.3638513381335,1.86523806059701,1.176489498967));
#13160=CARTESIAN_POINT('Ctrl Pts',(94.3597890157646,1.90425974664773,1.11223032996636));
#13161=CARTESIAN_POINT('Ctrl Pts',(94.3557266933958,1.93992218009633,1.04609652287459));
#13162=CARTESIAN_POINT('Ctrl Pts',(94.3516669492565,1.97556197970846,0.980004688851698));
#13163=CARTESIAN_POINT('Ctrl Pts',(94.3476072051172,2.00784653142256,0.912040996903966));
#13164=CARTESIAN_POINT('Ctrl Pts',(94.3435474609778,2.03658361171268,0.842581267595792));
#13165=CARTESIAN_POINT('Ctrl Pts',(94.3394889815228,2.0653117398788,0.77314317625862));
#13166=CARTESIAN_POINT('Ctrl Pts',(94.3354305020678,2.09049440834122,0.702210413774042));
#13167=CARTESIAN_POINT('Ctrl Pts',(94.3313720226127,2.11198706389033,0.630179848900211));
#13168=CARTESIAN_POINT('Ctrl Pts',(94.3273134959803,2.13347996927842,0.558148446715127));
#13169=CARTESIAN_POINT('Ctrl Pts',(94.3232549693479,2.15128264178525,0.485019674843072));
#13170=CARTESIAN_POINT('Ctrl Pts',(94.3191964427155,2.16530052215873,0.411205117598434));
#13171=CARTESIAN_POINT('Ctrl Pts',(94.3151337657304,2.17933273757372,0.337315075707495));
#13172=CARTESIAN_POINT('Ctrl Pts',(94.3110710887453,2.18957234255911,0.262738318103916));
#13173=CARTESIAN_POINT('Ctrl Pts',(94.3070084117602,2.19597616291718,0.187895428096429));
#13174=CARTESIAN_POINT('Ctrl Pts',(94.3029436127832,2.20238332807852,0.113013446620275));
#13175=CARTESIAN_POINT('Ctrl Pts',(94.2988788138061,2.20495070255364,0.0378655335523711));
#13176=CARTESIAN_POINT('Ctrl Pts',(94.2948140148291,2.20368727908339,-0.0371264865839261));
#13177=CARTESIAN_POINT('Ctrl Pts',(94.2907419545871,2.20242159866202,-0.112252470769029));
#13178=CARTESIAN_POINT('Ctrl Pts',(94.2866698943451,2.19731148395123,-0.187221528710871));
#13179=CARTESIAN_POINT('Ctrl Pts',(94.282597834103,2.18841791692943,-0.261616170873024));
#13180=CARTESIAN_POINT('Ctrl Pts',(94.2794596833042,2.18156405112303,-0.318948722912514));
#13181=CARTESIAN_POINT('Ctrl Pts',(94.2763215325053,2.17246423506766,-0.375940200071185));
#13182=CARTESIAN_POINT('Ctrl Pts',(94.2731833817064,2.16116682758316,-0.432404837338979));
#13183=CARTESIAN_POINT('Ctrl Pts',(94.2691103167704,2.14650370995695,-0.505691351887988));
#13184=CARTESIAN_POINT('Ctrl Pts',(94.2650372518344,2.12808030290967,-0.578372495913159));
#13185=CARTESIAN_POINT('Ctrl Pts',(94.2609641868984,2.10596124041854,-0.650033271344486));
#13186=CARTESIAN_POINT('Ctrl Pts',(94.2568971060934,2.08387467516676,-0.721588763047257));
#13187=CARTESIAN_POINT('Ctrl Pts',(94.2528300252883,2.0581033741769,-0.79212641008916));
#13188=CARTESIAN_POINT('Ctrl Pts',(94.2487629444833,2.02876296428268,-0.861241449742725));
#13189=CARTESIAN_POINT('Ctrl Pts',(94.2447006221144,1.99945688231918,-0.930275625621683));
#13190=CARTESIAN_POINT('Ctrl Pts',(94.2406382997456,1.96659017347895,-0.997890063672327));
#13191=CARTESIAN_POINT('Ctrl Pts',(94.2365759773767,1.93032773015936,-1.0636967867667));
#13192=CARTESIAN_POINT('Ctrl Pts',(94.2325162332374,1.89408830148383,-1.12946174438226));
#13193=CARTESIAN_POINT('Ctrl Pts',(94.2284564890981,1.85445764487347,-1.19342084662097));
#13194=CARTESIAN_POINT('Ctrl Pts',(94.2243967449588,1.81164748468374,-1.25520890342567));
#13195=CARTESIAN_POINT('Ctrl Pts',(94.2203382655037,1.76885066063877,-1.31697771212511));
#13196=CARTESIAN_POINT('Ctrl Pts',(94.2162797860487,1.72287657129991,-1.37657642598749));
#13197=CARTESIAN_POINT('Ctrl Pts',(94.2122213065936,1.67398046066359,-1.433668517237));
#13198=CARTESIAN_POINT('Ctrl Pts',(94.2081627799612,1.62508378163987,-1.49076127214717));
#13199=CARTESIAN_POINT('Ctrl Pts',(94.2041042533288,1.57326532581928,-1.54534698511569));
#13200=CARTESIAN_POINT('Ctrl Pts',(94.2000457266964,1.51881979329052,-1.59712317480805));
#13201=CARTESIAN_POINT('Ctrl Pts',(94.1959830497113,1.46431858337352,-1.64895231215068));
#13202=CARTESIAN_POINT('Ctrl Pts',(94.1919203727262,1.40718527868952,-1.69796585906177));
#13203=CARTESIAN_POINT('Ctrl Pts',(94.1878576957411,1.34774998440714,-1.74389964720753));
#13204=CARTESIAN_POINT('Ctrl Pts',(94.1837928967641,1.28828364625489,-1.78985742720123));
#13205=CARTESIAN_POINT('Ctrl Pts',(94.179728097787,1.22651331672078,-1.83273197255615));
#13206=CARTESIAN_POINT('Ctrl Pts',(94.17566329881,1.16279840932539,-1.87230228843271));
#13207=CARTESIAN_POINT('Ctrl Pts',(94.171591238568,1.09896968306027,-1.9119432918267));
#13208=CARTESIAN_POINT('Ctrl Pts',(94.167519178326,1.03318985897519,-1.94826804460465));
#13209=CARTESIAN_POINT('Ctrl Pts',(94.163447118084,0.965842875895455,-1.98110159736496));
#13210=CARTESIAN_POINT('Ctrl Pts',(94.1603089672851,0.913941632742322,-2.00640491649622));
#13211=CARTESIAN_POINT('Ctrl Pts',(94.1571708164862,0.861110159100261,-2.02963572607796));
#13212=CARTESIAN_POINT('Ctrl Pts',(94.1540326656873,0.807530791185746,-2.05073402012229));
#13213=CARTESIAN_POINT('Ctrl Pts',(94.1499596007513,0.737989121989469,-2.07811789272372));
#13214=CARTESIAN_POINT('Ctrl Pts',(94.1458865358153,0.666918861211004,-2.10201326166652));
#13215=CARTESIAN_POINT('Ctrl Pts',(94.1418134708793,0.59470383234052,-2.12224959696062));
#13216=CARTESIAN_POINT('Ctrl Pts',(94.1377463900743,0.522594901505407,-2.14245620111078));
#13217=CARTESIAN_POINT('Ctrl Pts',(94.1336793092692,0.449344997747966,-2.15901431708036));
#13218=CARTESIAN_POINT('Ctrl Pts',(94.1296122284641,0.375356970788698,-2.17180181979856));
#13219=CARTESIAN_POINT('Ctrl Pts',(94.1255499060953,0.301455508941461,-2.18457436129059));
#13220=CARTESIAN_POINT('Ctrl Pts',(94.1214875837264,0.226818107780517,-2.19358497341288));
#13221=CARTESIAN_POINT('Ctrl Pts',(94.1174252613575,0.151860201920908,-2.19876203329795));
#13222=CARTESIAN_POINT('Ctrl Pts',(94.1133655172182,0.0769498695110541,
-2.20393580746425));
#13223=CARTESIAN_POINT('Ctrl Pts',(94.1093057730789,0.00171991117514311,
-2.20528082467623));
#13224=CARTESIAN_POINT('Ctrl Pts',(94.1052460289396,-0.0734080163565206,
-2.2027771705587));
#13225=CARTESIAN_POINT('Ctrl Pts',(94.1011875494846,-0.148512540170232,
-2.20027429637503));
#13226=CARTESIAN_POINT('Ctrl Pts',(94.0971290700296,-0.223514619401914,
-2.19392514718078));
#13227=CARTESIAN_POINT('Ctrl Pts',(94.0930705905745,-0.297993107967888,
-2.18376191641938));
#13228=CARTESIAN_POINT('Ctrl Pts',(94.0890120639421,-0.372472462300833,
-2.17359856751663));
#13229=CARTESIAN_POINT('Ctrl Pts',(94.0849535373097,-0.44642774104921,-2.15962111534711));
#13230=CARTESIAN_POINT('Ctrl Pts',(94.0808950106773,-0.519445035845304,
-2.14191336303214));
#13231=CARTESIAN_POINT('Ctrl Pts',(94.0768323336922,-0.592536999986773,
-2.12418750231866));
#13232=CARTESIAN_POINT('Ctrl Pts',(94.0727696567071,-0.664688599654287,
-2.102723836501));
#13233=CARTESIAN_POINT('Ctrl Pts',(94.068706979722,-0.735498945136245,-2.07765668523543));
#13234=CARTESIAN_POINT('Ctrl Pts',(94.064642180745,-0.806346275833395,-2.05257644105275));
#13235=CARTESIAN_POINT('Ctrl Pts',(94.060577381768,-0.875850515500875,-2.02388914563516));
#13236=CARTESIAN_POINT('Ctrl Pts',(94.0565125827909,-0.943631181632175,
-1.99177714442441));
#13237=CARTESIAN_POINT('Ctrl Pts',(94.0524405225489,-1.01153292961262,-1.9596077790609));
#13238=CARTESIAN_POINT('Ctrl Pts',(94.0483684623069,-1.07770453300776,-1.92400171461756));
#13239=CARTESIAN_POINT('Ctrl Pts',(94.0442964020649,-1.14179092192146,-1.88518685827632));
#13240=CARTESIAN_POINT('Ctrl Pts',(94.041158251266,-1.19117937410965,-1.85527402172717));
#13241=CARTESIAN_POINT('Ctrl Pts',(94.038020100467,-1.23932991199915,-1.82345640361977));
#13242=CARTESIAN_POINT('Ctrl Pts',(94.0348819496681,-1.28609330739947,-1.78985474401201));
#13243=CARTESIAN_POINT('Ctrl Pts',(94.0308088847321,-1.34678839769241,-1.74624251811552));
#13244=CARTESIAN_POINT('Ctrl Pts',(94.0267358197961,-1.40537964316221,-1.69945537695057));
#13245=CARTESIAN_POINT('Ctrl Pts',(94.0226627548601,-1.46151575089349,-1.64972352528848));
#13246=CARTESIAN_POINT('Ctrl Pts',(94.018595674055,-1.51756938367673,-1.60006473946667));
#13247=CARTESIAN_POINT('Ctrl Pts',(94.01452859325,-1.57117468582549,-1.54747014671698));
#13248=CARTESIAN_POINT('Ctrl Pts',(94.0104615124449,-1.62201073967655,-1.49221217002607));
#13249=CARTESIAN_POINT('Ctrl Pts',(94.006399190076,-1.67278731594906,-1.43701884451085));
#13250=CARTESIAN_POINT('Ctrl Pts',(94.0023368677071,-1.72080075940068,-1.37916867570505));
#13251=CARTESIAN_POINT('Ctrl Pts',(93.9982745453383,-1.76576578042336,-1.31897202725679));
#13252=CARTESIAN_POINT('Ctrl Pts',(93.9942148011989,-1.81070226354682,-1.25881358374756));
#13253=CARTESIAN_POINT('Ctrl Pts',(93.9901550570596,-1.85259387851181,-1.19631199738186));
#13254=CARTESIAN_POINT('Ctrl Pts',(93.9860953129203,-1.89119542512883,-1.13181087818229));
#13255=CARTESIAN_POINT('Ctrl Pts',(93.9820368334652,-1.92978494666091,-1.06732985225632));
#13256=CARTESIAN_POINT('Ctrl Pts',(93.9779783540101,-1.9650861897439,-1.00085093964909));
#13257=CARTESIAN_POINT('Ctrl Pts',(93.9739198745551,-1.99689802718692,-0.932745554273499));
#13258=CARTESIAN_POINT('Ctrl Pts',(93.9698613479227,-2.02871023442301,-0.864639377214648));
#13259=CARTESIAN_POINT('Ctrl Pts',(93.9658028212903,-2.05703275504176,-0.794907123201642));
#13260=CARTESIAN_POINT('Ctrl Pts',(93.9617442946579,-2.08171176103076,-0.723942086071967));
#13261=CARTESIAN_POINT('Ctrl Pts',(93.9576816176728,-2.10641600439989,-0.652904478287715));
#13262=CARTESIAN_POINT('Ctrl Pts',(93.9536189406876,-2.12746913544939,-0.580632021860763));
#13263=CARTESIAN_POINT('Ctrl Pts',(93.9495562637025,-2.14476683879704,-0.507534439419188));
#13264=CARTESIAN_POINT('Ctrl Pts',(93.9454914647255,-2.16207357697252,-0.434398677107195));
#13265=CARTESIAN_POINT('Ctrl Pts',(93.9414266657484,-2.17562089518297,-0.360437400620822));
#13266=CARTESIAN_POINT('Ctrl Pts',(93.9373618667714,-2.18535590048339,-0.286069201806934));
#13267=CARTESIAN_POINT('Ctrl Pts',(93.9332898065293,-2.19510829617712,-0.211568153324482));
#13268=CARTESIAN_POINT('Ctrl Pts',(93.9292177462873,-2.20103473834352,-0.136659207234329));
#13269=CARTESIAN_POINT('Ctrl Pts',(93.9251456860453,-2.20313439749033,-0.0617642825176407));
#13270=CARTESIAN_POINT('Ctrl Pts',(93.9220075352465,-2.20475250887302,-0.00404618557138921));
#13271=CARTESIAN_POINT('Ctrl Pts',(93.9188693844478,-2.20409893500785,0.0536635013265952));
#13272=CARTESIAN_POINT('Ctrl Pts',(93.9157312336491,-2.20119430231718,0.111173933304467));
#13273=CARTESIAN_POINT('Ctrl Pts',(93.9116581687131,-2.19742432492508,0.185817804477317));
#13274=CARTESIAN_POINT('Ctrl Pts',(93.9075851037772,-2.18984594332277,0.260413640529149));
#13275=CARTESIAN_POINT('Ctrl Pts',(93.9035120388412,-2.17846230557427,0.334541452128176));
#13276=CARTESIAN_POINT('Ctrl Pts',(93.8994449580361,-2.16709539262136,0.408560355439342));
#13277=CARTESIAN_POINT('Ctrl Pts',(93.8953778772311,-2.15193439514934,0.482112131492625));
#13278=CARTESIAN_POINT('Ctrl Pts',(93.891310796426,-2.13303440332286,0.554779446483994));
#13279=CARTESIAN_POINT('Ctrl Pts',(93.8872484740572,-2.11415652426219,0.627361741580495));
#13280=CARTESIAN_POINT('Ctrl Pts',(93.8831861516883,-2.09154846171698,0.69906117177914));
#13281=CARTESIAN_POINT('Ctrl Pts',(93.8791238293194,-2.06531649876985,0.769469791420714));
#13282=CARTESIAN_POINT('Ctrl Pts',(93.8750640851802,-2.03910118443314,0.83983372490286));
#13283=CARTESIAN_POINT('Ctrl Pts',(93.8710043410409,-2.00926670002053,0.908908027232522));
#13284=CARTESIAN_POINT('Ctrl Pts',(93.8669445969016,-1.97596899326979,0.976300434106421));
#13285=CARTESIAN_POINT('Ctrl Pts',(93.8628861174465,-1.94268165936119,1.04367184701807));
#13286=CARTESIAN_POINT('Ctrl Pts',(93.8588276379915,-1.90593345650014,1.10936197695432));
#13287=CARTESIAN_POINT('Ctrl Pts',(93.8547691585364,-1.8659275810886,1.17300053799342));
#13288=CARTESIAN_POINT('Ctrl Pts',(93.8507106319041,-1.82592124063332,1.23663983879172));
#13289=CARTESIAN_POINT('Ctrl Pts',(93.8466521052717,-1.78265740806778,1.29822712007275));
#13290=CARTESIAN_POINT('Ctrl Pts',(93.8425935786393,-1.73638329740971,1.35741999560807));
#13291=CARTESIAN_POINT('Ctrl Pts',(93.8385309016542,-1.69006186566747,1.41667340328554));
#13292=CARTESIAN_POINT('Ctrl Pts',(93.8344682246692,-1.64072430318569,1.47352713854738));
#13293=CARTESIAN_POINT('Ctrl Pts',(93.8304055476841,-1.58865845924492,1.52767152878803));
#13294=CARTESIAN_POINT('Ctrl Pts',(93.826340748707,-1.53656542059916,1.58184419938694));
#13295=CARTESIAN_POINT('Ctrl Pts',(93.82227594973,-1.48174161115821,1.63330437980348));
#13296=CARTESIAN_POINT('Ctrl Pts',(93.8182111507529,-1.42451019646175,1.68178081216802));
#13297=CARTESIAN_POINT('Ctrl Pts',(93.8141390905109,-1.36717654486046,1.73034384173495));
#13298=CARTESIAN_POINT('Ctrl Pts',(93.810067030269,-1.30742707751986,1.77591218681686));
#13299=CARTESIAN_POINT('Ctrl Pts',(93.805994970027,-1.2456159654642,1.81825654586494));
#13300=CARTESIAN_POINT('Ctrl Pts',(93.8028568192279,-1.19798096520409,1.85088940890829));
#13301=CARTESIAN_POINT('Ctrl Pts',(93.7997186684289,-1.14912218783894,1.88160837691966));
#13302=CARTESIAN_POINT('Ctrl Pts',(93.7965805176298,-1.09921121319741,1.91032738261825));
#13303=CARTESIAN_POINT('Ctrl Pts',(93.7923397722511,-1.0317639333775,1.94913685944001));
#13304=CARTESIAN_POINT('Ctrl Pts',(93.7880990268724,-0.962152378046453,
1.98443203271001));
#13305=CARTESIAN_POINT('Ctrl Pts',(93.7838582814936,-0.890761497316347,
2.01597617914963));
#13306=CARTESIAN_POINT('Ctrl Pts',(93.7796285982377,-0.819556842030956,
2.04743804165272));
#13307=CARTESIAN_POINT('Ctrl Pts',(93.7753989149819,-0.746582486492347,
2.07516819060959));
#13308=CARTESIAN_POINT('Ctrl Pts',(93.771169231726,-0.672247882970542,2.09897565108355));
#13309=CARTESIAN_POINT('Ctrl Pts',(93.7669460737044,-0.598027957232878,
2.12274638321454));
#13310=CARTESIAN_POINT('Ctrl Pts',(93.7627229156828,-0.522452354479371,
2.14260632975068));
#13311=CARTESIAN_POINT('Ctrl Pts',(93.7584997576612,-0.445950619526727,
2.15841238991619));
#13312=CARTESIAN_POINT('Ctrl Pts',(93.7542842631783,-0.369587708175099,
2.17418976767089));
#13313=CARTESIAN_POINT('Ctrl Pts',(93.7500687686954,-0.292302421946365,
2.18592782015334));
#13314=CARTESIAN_POINT('Ctrl Pts',(93.7458532742125,-0.214538074458878,
2.19353354535723));
#13315=CARTESIAN_POINT('Ctrl Pts',(93.741987131945,-0.143218320170691,2.20050895851572));
#13316=CARTESIAN_POINT('Ctrl Pts',(93.7381209896775,-0.071496035973098,
2.20400907678262));
#13317=CARTESIAN_POINT('Ctrl Pts',(93.73425484741,0.00027926351991633,2.2039999823076));
#13318=CARTESIAN_POINT('',(92.9842548474409,0.00188421767977092,2.20399919458328));
#13319=CARTESIAN_POINT('Ctrl Pts',(93.734254847381,0.00027926405938751,
2.20399998230753));
#13320=CARTESIAN_POINT('Ctrl Pts',(93.7299610335033,0.0799943277350516,
2.20398988178464));
#13321=CARTESIAN_POINT('Ctrl Pts',(93.7256672196257,0.15960883666517,2.19965076805581));
#13322=CARTESIAN_POINT('Ctrl Pts',(93.7213734057481,0.23865534179794,2.19104076361699));
#13323=CARTESIAN_POINT('Ctrl Pts',(93.7170655055175,0.3179611681322,2.18240251306289));
#13324=CARTESIAN_POINT('Ctrl Pts',(93.7127576052869,0.396694877691193,2.16946540440215));
#13325=CARTESIAN_POINT('Ctrl Pts',(93.7084497050562,0.474397220033825,2.15233902478773));
#13326=CARTESIAN_POINT('Ctrl Pts',(93.7041342620763,0.552235612252334,2.13518265840906));
#13327=CARTESIAN_POINT('Ctrl Pts',(93.6998188190963,0.629038661404861,2.11382249435064));
#13328=CARTESIAN_POINT('Ctrl Pts',(93.6955033761164,0.704363112905398,2.08841772765369));
#13329=CARTESIAN_POINT('Ctrl Pts',(93.6911756325087,0.779902267285068,2.06294054786319));
#13330=CARTESIAN_POINT('Ctrl Pts',(93.6868478889011,0.853954037648477,2.03339586354069));
#13331=CARTESIAN_POINT('Ctrl Pts',(93.6825201452935,0.926095192750267,1.99999092347062));
#13332=CARTESIAN_POINT('Ctrl Pts',(93.6808233640659,0.954379621961421,1.98689382707146));
#13333=CARTESIAN_POINT('Ctrl Pts',(93.6791265828383,0.982370638153006,1.97320382397862));
#13334=CARTESIAN_POINT('Ctrl Pts',(93.6774298016107,1.01004390129631,1.95893525096011));
#13335=CARTESIAN_POINT('Ctrl Pts',(93.6733567366746,1.07647261699902,1.92468403253235));
#13336=CARTESIAN_POINT('Ctrl Pts',(93.6692836717384,1.14128524091617,1.88698397410478));
#13337=CARTESIAN_POINT('Ctrl Pts',(93.6652106068023,1.20410054898345,1.84601134014332));
#13338=CARTESIAN_POINT('Ctrl Pts',(93.661143525997,1.26682356904803,1.80509890301399));
#13339=CARTESIAN_POINT('Ctrl Pts',(93.6570764451918,1.327554702752,1.76092369498526));
#13340=CARTESIAN_POINT('Ctrl Pts',(93.6530093643866,1.38593658953909,1.71370819271449));
#13341=CARTESIAN_POINT('Ctrl Pts',(93.6489470420176,1.4442501702127,1.66654793202006));
#13342=CARTESIAN_POINT('Ctrl Pts',(93.6448847196485,1.50021959541092,1.61635474297736));
#13343=CARTESIAN_POINT('Ctrl Pts',(93.6408223972795,1.55351719080458,1.56339385244879));
#13344=CARTESIAN_POINT('Ctrl Pts',(93.6367626531401,1.60678095987339,1.51046657454895));
#13345=CARTESIAN_POINT('Ctrl Pts',(93.6327029090006,1.65737592629956,1.45477541658576));
#13346=CARTESIAN_POINT('Ctrl Pts',(93.6286431648611,1.70500920283994,1.39662436547237));
#13347=CARTESIAN_POINT('Ctrl Pts',(93.6245846854059,1.75262764074699,1.3384914294707));
#13348=CARTESIAN_POINT('Ctrl Pts',(93.6205262059507,1.79728591823297,1.27790049089922));
#13349=CARTESIAN_POINT('Ctrl Pts',(93.6164677264955,1.83873067296567,1.21518949645527));
#13350=CARTESIAN_POINT('Ctrl Pts',(93.612409199863,1.88017590946827,1.1524777730344));
#13351=CARTESIAN_POINT('Ctrl Pts',(93.6083506732304,1.91840728729221,1.08764634412842));
#13352=CARTESIAN_POINT('Ctrl Pts',(93.6042921465978,1.95321502813759,1.02106172872038));
#13353=CARTESIAN_POINT('Ctrl Pts',(93.6002294696126,1.98805836426528,0.954409022188786));
#13354=CARTESIAN_POINT('Ctrl Pts',(93.5961667926273,2.01947085023301,0.885999973001929));
#13355=CARTESIAN_POINT('Ctrl Pts',(93.5921041156421,2.0472892798299,0.81622460431769));
#13356=CARTESIAN_POINT('Ctrl Pts',(93.5880393166649,2.07512223937437,0.746412791000746));
#13357=CARTESIAN_POINT('Ctrl Pts',(93.5839745176877,2.09935725020407,0.675233689428349));
#13358=CARTESIAN_POINT('Ctrl Pts',(93.5799097187105,2.11988067472745,0.603093628649058));
#13359=CARTESIAN_POINT('Ctrl Pts',(93.5758376584683,2.14044076183223,0.530824698496752));
#13360=CARTESIAN_POINT('Ctrl Pts',(93.5717655982262,2.15727591200396,0.457591846304882));
#13361=CARTESIAN_POINT('Ctrl Pts',(93.567693537984,2.17032350217403,0.383812318602512));
#13362=CARTESIAN_POINT('Ctrl Pts',(93.5645553871865,2.18037868384186,0.326953807203578));
#13363=CARTESIAN_POINT('Ctrl Pts',(93.5614172363891,2.18818545146171,0.269770859593916));
#13364=CARTESIAN_POINT('Ctrl Pts',(93.5582790855916,2.19373625409253,0.212455283483507));
#13365=CARTESIAN_POINT('Ctrl Pts',(93.5542060206558,2.20094074521493,0.13806431937878));
#13366=CARTESIAN_POINT('Ctrl Pts',(93.55013295572,2.20437087458598,0.0631630187489451));
#13367=CARTESIAN_POINT('Ctrl Pts',(93.5460598907842,2.20396823644446,-0.0118326980817148));
#13368=CARTESIAN_POINT('Ctrl Pts',(93.5419928099794,2.20356618985732,-0.0867182315011731));
#13369=CARTESIAN_POINT('Ctrl Pts',(93.5379257291745,2.19934255830485,-0.161697432223492));
#13370=CARTESIAN_POINT('Ctrl Pts',(93.5338586483697,2.19129070684363,-0.236349398350684));
#13371=CARTESIAN_POINT('Ctrl Pts',(93.529796326001,2.1832482759529,-0.310914022565039));
#13372=CARTESIAN_POINT('Ctrl Pts',(93.5257340036323,2.17138657479198,-0.385151700518907));
#13373=CARTESIAN_POINT('Ctrl Pts',(93.5216716812637,2.15575098432446,-0.458643318477556));
#13374=CARTESIAN_POINT('Ctrl Pts',(93.5176119371246,2.14012531727954,-0.532088293593804));
#13375=CARTESIAN_POINT('Ctrl Pts',(93.5135521929855,2.12073061298998,-0.604787682501735));
#13376=CARTESIAN_POINT('Ctrl Pts',(93.5094924488463,2.09766367837493,-0.676330608819784));
#13377=CARTESIAN_POINT('Ctrl Pts',(93.5054339693915,2.0746039295302,-0.747851248213083));
#13378=CARTESIAN_POINT('Ctrl Pts',(93.5013754899366,2.04787436807721,-0.818215686167462));
#13379=CARTESIAN_POINT('Ctrl Pts',(93.4973170104818,2.01762175934515,-0.887027866651888));
#13380=CARTESIAN_POINT('Ctrl Pts',(93.4932584838496,1.98736879894502,-0.955840847035797));
#13381=CARTESIAN_POINT('Ctrl Pts',(93.4891999572174,1.95359290375311,-1.02310109775934));
#13382=CARTESIAN_POINT('Ctrl Pts',(93.4851414305852,1.91648846866269,-1.0884337138673));
#13383=CARTESIAN_POINT('Ctrl Pts',(93.4810787536003,1.87934608963182,-1.15383314077262));
#13384=CARTESIAN_POINT('Ctrl Pts',(93.4770160766154,1.83886860972418,-1.21730058049374));
#13385=CARTESIAN_POINT('Ctrl Pts',(93.4729533996305,1.79529541266976,-1.27848753660211));
#13386=CARTESIAN_POINT('Ctrl Pts',(93.4688886006536,1.75169945673649,-1.33970645149742));
#13387=CARTESIAN_POINT('Ctrl Pts',(93.4648238016767,1.70500486046904,-1.39864213618045));
#13388=CARTESIAN_POINT('Ctrl Pts',(93.4607590026999,1.6554915698996,-1.45497892149383));
#13389=CARTESIAN_POINT('Ctrl Pts',(93.4566869424581,1.60588982990756,-1.51141634556652));
#13390=CARTESIAN_POINT('Ctrl Pts',(93.4526148822162,1.55345967172619,-1.56524525446865));
#13391=CARTESIAN_POINT('Ctrl Pts',(93.4485428219744,1.4985178581826,-1.61618694113888));
#13392=CARTESIAN_POINT('Ctrl Pts',(93.4454046711738,1.45617671244284,-1.65544537183887));
#13393=CARTESIAN_POINT('Ctrl Pts',(93.4422665203731,1.41234464305599,-1.69298980974854));
#13394=CARTESIAN_POINT('Ctrl Pts',(93.4391283695725,1.3671787720371,-1.72870998299054));
#13395=CARTESIAN_POINT('Ctrl Pts',(93.4350553046367,1.30855713871575,-1.77507186754473));
#13396=CARTESIAN_POINT('Ctrl Pts',(93.4309822397009,1.24746154382153,-1.81853793371124));
#13397=CARTESIAN_POINT('Ctrl Pts',(93.4269091747651,1.18420992053786,-1.85883373761607));
#13398=CARTESIAN_POINT('Ctrl Pts',(93.4228420939602,1.12105122628956,-1.89907033908478));
#13399=CARTESIAN_POINT('Ctrl Pts',(93.4187750131553,1.05574319202988,-1.93614567138971));
#13400=CARTESIAN_POINT('Ctrl Pts',(93.4147079323504,0.988635988417915,-1.96982610461049));
#13401=CARTESIAN_POINT('Ctrl Pts',(93.4106456099818,0.921607299436438,-2.00346713212477));
#13402=CARTESIAN_POINT('Ctrl Pts',(93.4065832876131,0.852784047856998,-2.03372093889994));
#13403=CARTESIAN_POINT('Ctrl Pts',(93.4025209652444,0.78254308468408,-2.06039858294776));
#13404=CARTESIAN_POINT('Ctrl Pts',(93.3984612211053,0.712346701264204,-2.08705929552526));
#13405=CARTESIAN_POINT('Ctrl Pts',(93.3944014769662,0.640734836982481,-2.11014818021287));
#13406=CARTESIAN_POINT('Ctrl Pts',(93.3903417328271,0.568105283034198,-2.12952398140726));
#13407=CARTESIAN_POINT('Ctrl Pts',(93.3862832533722,0.495498354515015,-2.14889374668663));
#13408=CARTESIAN_POINT('Ctrl Pts',(93.3822247739173,0.42187482680223,-2.16455260204706));
#13409=CARTESIAN_POINT('Ctrl Pts',(93.3781662944625,0.347647103164469,-2.17640931160969));
#13410=CARTESIAN_POINT('Ctrl Pts',(93.3741077678303,0.273418516674914,-2.1882661589993));
#13411=CARTESIAN_POINT('Ctrl Pts',(93.3700492411981,0.198586192081613,-2.19632069929357));
#13412=CARTESIAN_POINT('Ctrl Pts',(93.3659907145659,0.123570561972054,-2.20053318907348));
#13413=CARTESIAN_POINT('Ctrl Pts',(93.361928037581,0.0484782189684729,-2.20474998665274));
#13414=CARTESIAN_POINT('Ctrl Pts',(93.3578653605961,-0.0267973261153622,
-2.20511686094239));
#13415=CARTESIAN_POINT('Ctrl Pts',(93.3538026836112,-0.10183346103039,-2.20164619006201));
#13416=CARTESIAN_POINT('Ctrl Pts',(93.3497378846343,-0.176908788348498,
-2.1981737064026));
#13417=CARTESIAN_POINT('Ctrl Pts',(93.3456730856575,-0.251743980839748,
-2.1908597324871));
#13418=CARTESIAN_POINT('Ctrl Pts',(93.3416082866806,-0.325922039898365,
-2.17976852530458));
#13419=CARTESIAN_POINT('Ctrl Pts',(93.3375362264388,-0.400232608964159,
-2.16865750504037));
#13420=CARTESIAN_POINT('Ctrl Pts',(93.333464166197,-0.473883231174135,-2.15375586859984));
#13421=CARTESIAN_POINT('Ctrl Pts',(93.3293921059552,-0.546468026254893,
-2.13517884409739));
#13422=CARTESIAN_POINT('Ctrl Pts',(93.3262539551545,-0.60240581186443,-2.12086237998498));
#13423=CARTESIAN_POINT('Ctrl Pts',(93.3231158043539,-0.657710809498464,
-2.10436412670199));
#13424=CARTESIAN_POINT('Ctrl Pts',(93.3199776535533,-0.712205204349463,
-2.08575639682527));
#13425=CARTESIAN_POINT('Ctrl Pts',(93.3159045886161,-0.782934504196159,
-2.06160507429907));
#13426=CARTESIAN_POINT('Ctrl Pts',(93.3118315236789,-0.852570328624139,
-2.03380538754666));
#13427=CARTESIAN_POINT('Ctrl Pts',(93.3077584587417,-0.920709746421028,
-2.00247585824282));
#13428=CARTESIAN_POINT('Ctrl Pts',(93.3036913779354,-0.988749054054269,
-1.97119235815976));
#13429=CARTESIAN_POINT('Ctrl Pts',(93.2996242971292,-1.05529588980259,-1.93638950971336));
#13430=CARTESIAN_POINT('Ctrl Pts',(93.2955572163229,-1.11996415941918,-1.89823504382795));
#13431=CARTESIAN_POINT('Ctrl Pts',(93.2914948939528,-1.18455676792911,-1.86012521821403));
#13432=CARTESIAN_POINT('Ctrl Pts',(93.2874325715827,-1.24727476787778,-1.81867180739638));
#13433=CARTESIAN_POINT('Ctrl Pts',(93.2833702492127,-1.30775516900774,-1.77408917981412));
#13434=CARTESIAN_POINT('Ctrl Pts',(93.2793105050721,-1.36819718510961,-1.72953484743792));
#13435=CARTESIAN_POINT('Ctrl Pts',(93.2752507609316,-1.42640403714235,-1.68185552191804));
#13436=CARTESIAN_POINT('Ctrl Pts',(93.2711910167911,-1.4820414691536,-1.63130900926497));
#13437=CARTESIAN_POINT('Ctrl Pts',(93.2671325373349,-1.53766156909124,-1.58077824277138));
#13438=CARTESIAN_POINT('Ctrl Pts',(93.2630740578786,-1.59071348504336,-1.52738238336798));
#13439=CARTESIAN_POINT('Ctrl Pts',(93.2590155784223,-1.64089708522505,-1.47141862014178));
#13440=CARTESIAN_POINT('Ctrl Pts',(93.2549570517888,-1.6910812687603,-1.41545420637117));
#13441=CARTESIAN_POINT('Ctrl Pts',(93.2508985251552,-1.73839675289855,-1.35692218617953));
#13442=CARTESIAN_POINT('Ctrl Pts',(93.2468399985216,-1.78258233451936,-1.29615439692172));
#13443=CARTESIAN_POINT('Ctrl Pts',(93.2427773215353,-1.82681310144118,-1.23532446497509));
#13444=CARTESIAN_POINT('Ctrl Pts',(93.238714644549,-1.86790729277984,-1.17225458526842));
#13445=CARTESIAN_POINT('Ctrl Pts',(93.2346519675628,-1.9056463322809,-1.10730666766906));
#13446=CARTESIAN_POINT('Ctrl Pts',(93.2305871685845,-1.94340508340016,-1.04232482688109));
#13447=CARTESIAN_POINT('Ctrl Pts',(93.2265223696063,-1.97780497422523,-0.975463419742705));
#13448=CARTESIAN_POINT('Ctrl Pts',(93.2224575706281,-2.00867407397818,-0.907107746923103));
#13449=CARTESIAN_POINT('Ctrl Pts',(93.2183855103849,-2.03959831759262,-0.838629965075903));
#13450=CARTESIAN_POINT('Ctrl Pts',(93.2143134501417,-2.06697899750677,-0.768653031078391));
#13451=CARTESIAN_POINT('Ctrl Pts',(93.2102413898986,-2.0906930480191,-0.697580517907859));
#13452=CARTESIAN_POINT('Ctrl Pts',(93.2071032391105,-2.10896838331895,-0.642808179115762));
#13453=CARTESIAN_POINT('Ctrl Pts',(93.2039650883223,-2.12506707995825,-0.587385556796277));
#13454=CARTESIAN_POINT('Ctrl Pts',(93.2008269375342,-2.13895357252642,-0.531501283701617));
#13455=CARTESIAN_POINT('Ctrl Pts',(93.1967538726001,-2.15697711242492,-0.458968034511747));
#13456=CARTESIAN_POINT('Ctrl Pts',(93.192680807666,-2.17134175589633,-0.385377086445622));
#13457=CARTESIAN_POINT('Ctrl Pts',(93.1886077427318,-2.18192880331932,-0.311131318329639));
#13458=CARTESIAN_POINT('Ctrl Pts',(93.1845406619286,-2.19250029629402,-0.236994631803124));
#13459=CARTESIAN_POINT('Ctrl Pts',(93.1804735811254,-2.19930514545084,-0.162205504061917));
#13460=CARTESIAN_POINT('Ctrl Pts',(93.1764065003222,-2.20227513387128,-0.0871793251420103));
#13461=CARTESIAN_POINT('Ctrl Pts',(93.1723441779552,-2.20524164744059,-0.0122409259592655));
#13462=CARTESIAN_POINT('Ctrl Pts',(93.1682818555882,-2.20438219561364,0.0629334986872736));
#13463=CARTESIAN_POINT('Ctrl Pts',(93.1642195332212,-2.19968027824874,0.137922708367928));
#13464=CARTESIAN_POINT('Ctrl Pts',(93.1601597890837,-2.19498134504443,0.212864324731502));
#13465=CARTESIAN_POINT('Ctrl Pts',(93.1561000449462,-2.18644481542838,0.287620484077586));
#13466=CARTESIAN_POINT('Ctrl Pts',(93.1520403008087,-2.17410626712244,0.361770561625636));
#13467=CARTESIAN_POINT('Ctrl Pts',(93.1479818213555,-2.16177156249902,0.435897540074029));
#13468=CARTESIAN_POINT('Ctrl Pts',(93.1439233419023,-2.14563726907795,0.509418340912239));
#13469=CARTESIAN_POINT('Ctrl Pts',(93.139864862449,-2.12579055500329,0.581919681965469));
#13470=CARTESIAN_POINT('Ctrl Pts',(93.1358063358184,-2.10594361022266,0.654421865802651));
#13471=CARTESIAN_POINT('Ctrl Pts',(93.1317478091879,-2.08238428689612,0.725904106280534));
#13472=CARTESIAN_POINT('Ctrl Pts',(93.1276892825573,-2.05524996718571,0.795967067398613));
#13473=CARTESIAN_POINT('Ctrl Pts',(93.1236266055739,-2.02808789922857,0.866101676685974));
#13474=CARTESIAN_POINT('Ctrl Pts',(93.1195639285906,-1.99734370711549,0.934813662042519));
#13475=CARTESIAN_POINT('Ctrl Pts',(93.1155012516073,-1.96320314489218,1.00172322119709));
#13476=CARTESIAN_POINT('Ctrl Pts',(93.111436452632,-1.92904475058451,1.06866772813299));
#13477=CARTESIAN_POINT('Ctrl Pts',(93.1073716536567,-1.8914866921888,1.13380752008037));
#13478=CARTESIAN_POINT('Ctrl Pts',(93.1033068546814,-1.85075965706099,1.19678932640439));
#13479=CARTESIAN_POINT('Ctrl Pts',(93.0992347944411,-1.80995986807815,1.2598836420037));
#13480=CARTESIAN_POINT('Ctrl Pts',(93.0951627342008,-1.76598007484198,1.32081188424882));
#13481=CARTESIAN_POINT('Ctrl Pts',(93.0910906739605,-1.71909279857905,1.37925195300701));
#13482=CARTESIAN_POINT('Ctrl Pts',(93.0879525231453,-1.68295891657785,1.42428904445179));
#13483=CARTESIAN_POINT('Ctrl Pts',(93.0848143723301,-1.64509912749844,1.46784902064739));
#13484=CARTESIAN_POINT('Ctrl Pts',(93.081676221515,-1.60565270601093,1.5097997839713));
#13485=CARTESIAN_POINT('Ctrl Pts',(93.0776169975952,-1.55462843500475,1.56406344176426));
#13486=CARTESIAN_POINT('Ctrl Pts',(93.0735577736755,-1.50073622542071,1.61585852701187));
#13487=CARTESIAN_POINT('Ctrl Pts',(93.0694985497557,-1.44424906282091,1.66486054807631));
#13488=CARTESIAN_POINT('Ctrl Pts',(93.0654926831042,-1.38850440685476,1.71321845242416));
#13489=CARTESIAN_POINT('Ctrl Pts',(93.0614868164527,-1.33023296663678,1.75885591939796));
#13490=CARTESIAN_POINT('Ctrl Pts',(93.0574809498012,-1.26973675548576,1.80149509346223));
#13491=CARTESIAN_POINT('Ctrl Pts',(93.0534789146843,-1.20929840779994,1.84409348397465));
#13492=CARTESIAN_POINT('Ctrl Pts',(93.0494768795674,-1.14663990856198,1.88369898483093));
#13493=CARTESIAN_POINT('Ctrl Pts',(93.0454748444505,-1.08209667048888,1.92007364330561));
#13494=CARTESIAN_POINT('Ctrl Pts',(93.0414752540233,-1.01759285940324,1.95642608189721));
#13495=CARTESIAN_POINT('Ctrl Pts',(93.0374756635961,-0.95120702175299,1.9895513517484));
#13496=CARTESIAN_POINT('Ctrl Pts',(93.0334760731688,-0.883302375358345,
2.01925553451917));
#13497=CARTESIAN_POINT('Ctrl Pts',(93.0293743043582,-0.813662954585416,
2.04971857633619));
#13498=CARTESIAN_POINT('Ctrl Pts',(93.0252725355475,-0.742426518699399,
2.07658305520151));
#13499=CARTESIAN_POINT('Ctrl Pts',(93.0211707667368,-0.670008820827188,
2.09969144876426));
#13500=CARTESIAN_POINT('Ctrl Pts',(93.0171702427475,-0.599378624206823,
2.12222945299353));
#13501=CARTESIAN_POINT('Ctrl Pts',(93.0131697187582,-0.527625316494081,
2.14119457669626));
#13502=CARTESIAN_POINT('Ctrl Pts',(93.0091691947689,-0.455149799192628,
2.15649128453952));
#13503=CARTESIAN_POINT('Ctrl Pts',(93.0050168035476,-0.379922978253986,
2.17236868348363));
#13504=CARTESIAN_POINT('Ctrl Pts',(93.0008644123262,-0.30391857829625,2.18429343026794));
#13505=CARTESIAN_POINT('Ctrl Pts',(92.9967120211049,-0.227593599682892,
2.19221740559265));
#13506=CARTESIAN_POINT('Ctrl Pts',(92.9925596298835,-0.151268621069534,
2.20014138091737));
#13507=CARTESIAN_POINT('Ctrl Pts',(92.9884072386622,-0.0746236549780797,
2.20406460181512));
#13508=CARTESIAN_POINT('Ctrl Pts',(92.9842548474409,0.00188421767977065,
2.20399919458328));
#13509=CARTESIAN_POINT('',(92.2342548473559,-0.00137440680590686,2.20399957146228));
#13510=CARTESIAN_POINT('Ctrl Pts',(92.98425484741,0.00188421824854456,2.20399919458279));
#13511=CARTESIAN_POINT('Ctrl Pts',(92.9781257762528,0.114812449383132,2.2039026512472));
#13512=CARTESIAN_POINT('Ctrl Pts',(92.9719967050956,0.227381640137665,2.19512359098658));
#13513=CARTESIAN_POINT('Ctrl Pts',(92.9658676339383,0.338536671029629,2.1778450179864));
#13514=CARTESIAN_POINT('Ctrl Pts',(92.9647535911242,0.358740623674827,2.17470440016757));
#13515=CARTESIAN_POINT('Ctrl Pts',(92.96363954831,0.378897939605397,2.17128308505399));
#13516=CARTESIAN_POINT('Ctrl Pts',(92.9625255054959,0.399002376888916,2.16758231752268));
#13517=CARTESIAN_POINT('Ctrl Pts',(92.9584524405509,0.472506444865692,2.15405189812562));
#13518=CARTESIAN_POINT('Ctrl Pts',(92.9543793756058,0.545463242913075,2.13675229502994));
#13519=CARTESIAN_POINT('Ctrl Pts',(92.9503063106608,0.61745682495046,2.11574173029746));
#13520=CARTESIAN_POINT('Ctrl Pts',(92.9462392298466,0.689344634301983,2.09476203420356));
#13521=CARTESIAN_POINT('Ctrl Pts',(92.9421721490325,0.76027158276383,2.07008233382741));
#13522=CARTESIAN_POINT('Ctrl Pts',(92.9381050682184,0.829831171461187,2.04181199596617));
#13523=CARTESIAN_POINT('Ctrl Pts',(92.9340427458404,0.899309376266912,2.01357473406407));
#13524=CARTESIAN_POINT('Ctrl Pts',(92.9299804234625,0.967422959632449,1.98175535997734));
#13525=CARTESIAN_POINT('Ctrl Pts',(92.9259181010845,1.0337814460212,1.9465127592344));
#13526=CARTESIAN_POINT('Ctrl Pts',(92.9218583569362,1.10009781674412,1.91129252587319));
#13527=CARTESIAN_POINT('Ctrl Pts',(92.9177986127878,1.16466088030358,1.87265360056057));
#13528=CARTESIAN_POINT('Ctrl Pts',(92.9137388686394,1.22710222281299,1.83080204685472));
#13529=CARTESIAN_POINT('Ctrl Pts',(92.9096803891753,1.28952411370656,1.78896353067036));
#13530=CARTESIAN_POINT('Ctrl Pts',(92.9056219097112,1.34982519949281,1.74391463878128));
#13531=CARTESIAN_POINT('Ctrl Pts',(92.9015634302472,1.40766505356151,1.69590539151854));
#13532=CARTESIAN_POINT('Ctrl Pts',(92.8975049036057,1.46550557998272,1.64789558617803));
#13533=CARTESIAN_POINT('Ctrl Pts',(92.8934463769643,1.52088445163445,1.59692566346434));
#13534=CARTESIAN_POINT('Ctrl Pts',(92.8893878503229,1.57349467541003,1.54328562050461));
#13535=CARTESIAN_POINT('Ctrl Pts',(92.885325173329,1.6261586997389,1.48959072387229));
#13536=CARTESIAN_POINT('Ctrl Pts',(92.8812624963349,1.67604808719716,1.43322059590487));
#13537=CARTESIAN_POINT('Ctrl Pts',(92.8771998193409,1.72289360674796,1.37450122583685));
#13538=CARTESIAN_POINT('Ctrl Pts',(92.873135020355,1.76976359435597,1.31575118583668));
#13539=CARTESIAN_POINT('Ctrl Pts',(92.8690702213691,1.81358626948841,1.25464984855142));
#13540=CARTESIAN_POINT('Ctrl Pts',(92.8650054223832,1.85413511717714,1.19155317432774));
#13541=CARTESIAN_POINT('Ctrl Pts',(92.8609333621325,1.89475640040844,1.12834378563517));
#13542=CARTESIAN_POINT('Ctrl Pts',(92.8568613018818,1.93209193710563,1.06313235531274));
#13543=CARTESIAN_POINT('Ctrl Pts',(92.8527892416311,1.96596087378275,0.996300076661332));
#13544=CARTESIAN_POINT('Ctrl Pts',(92.849651090913,1.99206211527021,0.944795494132873));
#13545=CARTESIAN_POINT('Ctrl Pts',(92.8465129401949,2.01610544935589,0.892328809120288));
#13546=CARTESIAN_POINT('Ctrl Pts',(92.8433747894768,2.03802806340256,0.83908141010489));
#13547=CARTESIAN_POINT('Ctrl Pts',(92.8393017245573,2.06648183705378,0.769970608086717));
#13548=CARTESIAN_POINT('Ctrl Pts',(92.8352286596379,2.0914711115984,0.69927756218022));
#13549=CARTESIAN_POINT('Ctrl Pts',(92.8311555947184,2.1128194542164,0.627383418560555));
#13550=CARTESIAN_POINT('Ctrl Pts',(92.8270885139298,2.13413643193369,0.555594901532919));
#13551=CARTESIAN_POINT('Ctrl Pts',(92.8230214331413,2.15182296336987,0.482609244246773));
#13552=CARTESIAN_POINT('Ctrl Pts',(92.8189543523527,2.16575072124869,0.40882736382337));
#13553=CARTESIAN_POINT('Ctrl Pts',(92.8148920300002,2.17966218381672,0.335131807321105));
#13554=CARTESIAN_POINT('Ctrl Pts',(92.8108297076477,2.18982352197309,0.260642345318643));
#13555=CARTESIAN_POINT('Ctrl Pts',(92.8067673852952,2.19615671042189,0.185773257679682));
#13556=CARTESIAN_POINT('Ctrl Pts',(92.8027076411722,2.20248587939321,0.110951687118969));
#13557=CARTESIAN_POINT('Ctrl Pts',(92.7986478970492,2.20499167980752,0.0357514435901753));
#13558=CARTESIAN_POINT('Ctrl Pts',(92.7945881529262,2.20364769268452,-0.039406173706866));
#13559=CARTESIAN_POINT('Ctrl Pts',(92.7905296734873,2.20230412423795,-0.114540378038851));
#13560=CARTESIAN_POINT('Ctrl Pts',(92.7864711940484,2.19711315790207,-0.18963150543074));
#13561=CARTESIAN_POINT('Ctrl Pts',(92.7824127146095,2.18810048419052,-0.264257963144402));
#13562=CARTESIAN_POINT('Ctrl Pts',(92.7783541879932,2.17908770571187,-0.338885288347263));
#13563=CARTESIAN_POINT('Ctrl Pts',(92.7742956613769,2.16625319067707,-0.413047459345614));
#13564=CARTESIAN_POINT('Ctrl Pts',(92.7702371347605,2.14967434482391,-0.486329323818632));
#13565=CARTESIAN_POINT('Ctrl Pts',(92.7661744577912,2.1330785450194,-0.559686128198569));
#13566=CARTESIAN_POINT('Ctrl Pts',(92.7621117808218,2.11273087359491,-0.632160361630832));
#13567=CARTESIAN_POINT('Ctrl Pts',(92.7580491038525,2.08875944771065,-0.703349109332978));
#13568=CARTESIAN_POINT('Ctrl Pts',(92.753984304891,2.06477550122077,-0.774575039897725));
#13569=CARTESIAN_POINT('Ctrl Pts',(92.7499195059296,2.03716420656243,-0.844513703133851));
#13570=CARTESIAN_POINT('Ctrl Pts',(92.7458547069682,2.00610201588495,-0.912781847903619));
#13571=CARTESIAN_POINT('Ctrl Pts',(92.7417826467414,1.97498433640915,-0.981171945350702));
#13572=CARTESIAN_POINT('Ctrl Pts',(92.7377105865146,1.94040366765108,-1.047885139144));
#13573=CARTESIAN_POINT('Ctrl Pts',(92.7336385262877,1.90258241024026,-1.11256288462467));
#13574=CARTESIAN_POINT('Ctrl Pts',(92.7305003753443,1.87343529354423,-1.16240707078391));
#13575=CARTESIAN_POINT('Ctrl Pts',(92.727362224401,1.84236451852845,-1.21104288439625));
#13576=CARTESIAN_POINT('Ctrl Pts',(92.7242240734576,1.8094885080123,-1.25831925176857));
#13577=CARTESIAN_POINT('Ctrl Pts',(92.7201510085218,1.76681811768437,-1.31968013520277));
#13578=CARTESIAN_POINT('Ctrl Pts',(92.716077943586,1.72094072377547,-1.37898641940612));
#13579=CARTESIAN_POINT('Ctrl Pts',(92.7120048786501,1.67208108251626,-1.43588330079128));
#13580=CARTESIAN_POINT('Ctrl Pts',(92.7079377978454,1.62329322565133,-1.49269658950033));
#13581=CARTESIAN_POINT('Ctrl Pts',(92.7038707170407,1.57153212899213,-1.54710714428562));
#13582=CARTESIAN_POINT('Ctrl Pts',(92.6998036362361,1.51706523070615,-1.5987898816863));
#13583=CARTESIAN_POINT('Ctrl Pts',(92.6957413138678,1.4626620580471,-1.65041215089538));
#13584=CARTESIAN_POINT('Ctrl Pts',(92.6916789914996,1.405559718007,-1.69931261653392));
#13585=CARTESIAN_POINT('Ctrl Pts',(92.6876166691313,1.34606413470656,-1.7452012334561));
#13586=CARTESIAN_POINT('Ctrl Pts',(92.6835569249928,1.28660631140329,-1.79106072629965));
#13587=CARTESIAN_POINT('Ctrl Pts',(92.6794971808543,1.22475863607776,-1.83391187278125));
#13588=CARTESIAN_POINT('Ctrl Pts',(92.6754374367157,1.16086089392329,-1.87350419934401));
#13589=CARTESIAN_POINT('Ctrl Pts',(92.6713789572616,1.0969830570819,-1.91308419217431));
#13590=CARTESIAN_POINT('Ctrl Pts',(92.6673204778075,1.03105682698992,-1.94940712936845));
#13591=CARTESIAN_POINT('Ctrl Pts',(92.6632619983534,0.963450469551541,-1.98226617605228));
#13592=CARTESIAN_POINT('Ctrl Pts',(92.6592034717221,0.895843326233218,-2.01512560470116));
#13593=CARTESIAN_POINT('Ctrl Pts',(92.6551449450908,0.826556446999674,-2.04452085578788));
#13594=CARTESIAN_POINT('Ctrl Pts',(92.6510864184595,0.755980704991898,-2.07029205033492));
#13595=CARTESIAN_POINT('Ctrl Pts',(92.6470237414757,0.685332790436652,-2.09608959916048));
#13596=CARTESIAN_POINT('Ctrl Pts',(92.6429610644919,0.613393830580244,-2.11825552653667));
#13597=CARTESIAN_POINT('Ctrl Pts',(92.6388983875081,0.540571889473374,-2.13667920669229));
#13598=CARTESIAN_POINT('Ctrl Pts',(92.6348335885325,0.467711912469498,-2.15511250978833));
#13599=CARTESIAN_POINT('Ctrl Pts',(92.630768789557,0.393968504493352,-2.16979957986629));
#13600=CARTESIAN_POINT('Ctrl Pts',(92.6267039905813,0.31975939130576,-2.18068107059968));
#13601=CARTESIAN_POINT('Ctrl Pts',(92.622631930341,0.245417712640053,-2.19158199978153));
#13602=CARTESIAN_POINT('Ctrl Pts',(92.6185598701006,0.170609143097865,-2.19866372567662));
#13603=CARTESIAN_POINT('Ctrl Pts',(92.6144878098602,0.0957555386176693,
-2.20191890786742));
#13604=CARTESIAN_POINT('Ctrl Pts',(92.611349659053,0.0380692851103723,-2.20442752807849));
#13605=CARTESIAN_POINT('Ctrl Pts',(92.6082115082458,-0.0196436158345241,
-2.20466460375587));
#13606=CARTESIAN_POINT('Ctrl Pts',(92.6050733574385,-0.0771920237636312,
-2.20264781376126));
#13607=CARTESIAN_POINT('Ctrl Pts',(92.6010002924366,-0.151885185644805,
-2.20003018406536));
#13608=CARTESIAN_POINT('Ctrl Pts',(92.5969272274347,-0.226589089110338,
-2.19360386226274));
#13609=CARTESIAN_POINT('Ctrl Pts',(92.5928541624328,-0.300883746248021,
-2.18336551480593));
#13610=CARTESIAN_POINT('Ctrl Pts',(92.5887870815615,-0.375069249975267,
-2.17314220948788));
#13611=CARTESIAN_POINT('Ctrl Pts',(92.5847200006903,-0.448846232063083,
-2.15911806265758));
#13612=CARTESIAN_POINT('Ctrl Pts',(92.580652919819,-0.52179655824522,-2.14134171766289));
#13613=CARTESIAN_POINT('Ctrl Pts',(92.5765905973839,-0.594661533415905,
-2.12358617077979));
#13614=CARTESIAN_POINT('Ctrl Pts',(92.5725282749488,-0.666701312686266,
-2.10208726018484));
#13615=CARTESIAN_POINT('Ctrl Pts',(92.5684659525136,-0.737506358812478,
-2.07694496092486));
#13616=CARTESIAN_POINT('Ctrl Pts',(92.564406208308,-0.808266467180875,-2.05181861869925));
#13617=CARTESIAN_POINT('Ctrl Pts',(92.5603464641024,-0.877792948671281,
-2.02305363577183));
#13618=CARTESIAN_POINT('Ctrl Pts',(92.5562867198968,-0.94569117910778,-1.99079988792388));
#13619=CARTESIAN_POINT('Ctrl Pts',(92.5522282403755,-1.01356825800776,-1.95855618770635));
#13620=CARTESIAN_POINT('Ctrl Pts',(92.5481697608542,-1.07981766194409,-1.92282608512564));
#13621=CARTESIAN_POINT('Ctrl Pts',(92.544111281333,-1.14406601336773,-1.88380703816948));
#13622=CARTESIAN_POINT('Ctrl Pts',(92.5400527546345,-1.20831511163644,-1.84478753764241));
#13623=CARTESIAN_POINT('Ctrl Pts',(92.535994227936,-1.27056270404162,-1.80247926620495));
#13624=CARTESIAN_POINT('Ctrl Pts',(92.5319357012376,-1.33046263012875,-1.75712412476492));
#13625=CARTESIAN_POINT('Ctrl Pts',(92.5278730241872,-1.39042381139436,-1.71172260201083));
#13626=CARTESIAN_POINT('Ctrl Pts',(92.5238103471367,-1.44803215061752,-1.66326827603025));
#13627=CARTESIAN_POINT('Ctrl Pts',(92.5197476700863,-1.50297356999078,-1.61204418298916));
#13628=CARTESIAN_POINT('Ctrl Pts',(92.5156828710442,-1.55794368601694,-1.56079333490542));
#13629=CARTESIAN_POINT('Ctrl Pts',(92.5116180720021,-1.61024377582217,-1.50677018218588));
#13630=CARTESIAN_POINT('Ctrl Pts',(92.50755327296,-1.65959762676236,-1.45029366586383));
#13631=CARTESIAN_POINT('Ctrl Pts',(92.5034812126542,-1.70903964228944,-1.39371626118888));
#13632=CARTESIAN_POINT('Ctrl Pts',(92.4994091523483,-1.75552461052594,-1.33467711463645));
#13633=CARTESIAN_POINT('Ctrl Pts',(92.4953370920425,-1.7988177916779,-1.27352681649938));
#13634=CARTESIAN_POINT('Ctrl Pts',(92.4921989418348,-1.83218186176058,-1.22640108495611));
#13635=CARTESIAN_POINT('Ctrl Pts',(92.4890607916271,-1.86365115066336,-1.17802218742702));
#13636=CARTESIAN_POINT('Ctrl Pts',(92.4859226414194,-1.89313695359527,-1.12856035502406));
#13637=CARTESIAN_POINT('Ctrl Pts',(92.4818495766249,-1.93140713759191,-1.06436290273681));
#13638=CARTESIAN_POINT('Ctrl Pts',(92.4777765118305,-1.96648195830376,-0.998092794767605));
#13639=CARTESIAN_POINT('Ctrl Pts',(92.473703447036,-1.9981310558318,-0.930101222298135));
#13640=CARTESIAN_POINT('Ctrl Pts',(92.4696363663724,-2.02973365462996,-0.862209542780111));
#13641=CARTESIAN_POINT('Ctrl Pts',(92.4655692857087,-2.05792032310153,-0.792601849463247));
#13642=CARTESIAN_POINT('Ctrl Pts',(92.4615022050451,-2.08250539196889,-0.721655937701978));
#13643=CARTESIAN_POINT('Ctrl Pts',(92.4574398828168,-2.10706169660204,-0.650793031802234));
#13644=CARTESIAN_POINT('Ctrl Pts',(92.4533775605885,-2.12802461799624,-0.578595467019371));
#13645=CARTESIAN_POINT('Ctrl Pts',(92.4493152383602,-2.14525628891183,-0.505461625530791));
#13646=CARTESIAN_POINT('Ctrl Pts',(92.4452554943608,-2.16247702342434,-0.432374199806173));
#13647=CARTESIAN_POINT('Ctrl Pts',(92.4411957503615,-2.17597109749026,-0.358352140109323));
#13648=CARTESIAN_POINT('Ctrl Pts',(92.4371360063622,-2.18565066535416,-0.28380833151428));
#13649=CARTESIAN_POINT('Ctrl Pts',(92.4330775270464,-2.19532721785809,-0.20928774466007));
#13650=CARTESIAN_POINT('Ctrl Pts',(92.4290190477305,-2.20119156201161,-0.134246204789088));
#13651=CARTESIAN_POINT('Ctrl Pts',(92.4249605684147,-2.20320735648669,-0.0591045203256604));
#13652=CARTESIAN_POINT('Ctrl Pts',(92.4209020419205,-2.20522317439463,0.0160380376317814));
#13653=CARTESIAN_POINT('Ctrl Pts',(92.4168435154264,-2.20339034278361,0.0912802651559923));
#13654=CARTESIAN_POINT('Ctrl Pts',(92.4127849889322,-2.19772462112312,0.166200149546355));
#13655=CARTESIAN_POINT('Ctrl Pts',(92.4087223120829,-2.19205310554775,0.241196648966532));
#13656=CARTESIAN_POINT('Ctrl Pts',(92.4046596352336,-2.18254090876318,0.315869669828599));
#13657=CARTESIAN_POINT('Ctrl Pts',(92.4005969583843,-2.16925574722204,0.389801876783747));
#13658=CARTESIAN_POINT('Ctrl Pts',(92.3965321595419,-2.15596364665474,0.46377269956734));
#13659=CARTESIAN_POINT('Ctrl Pts',(92.3924673606996,-2.13889476541545,0.537001472467057));
#13660=CARTESIAN_POINT('Ctrl Pts',(92.3884025618572,-2.11816751391238,0.609083231591761));
#13661=CARTESIAN_POINT('Ctrl Pts',(92.3843305017464,-2.09740323569742,0.681293756005356));
#13662=CARTESIAN_POINT('Ctrl Pts',(92.3802584416357,-2.0729676890925,0.752352721743964));
#13663=CARTESIAN_POINT('Ctrl Pts',(92.3761863815249,-2.04502835636642,0.82187287438949));
#13664=CARTESIAN_POINT('Ctrl Pts',(92.3730482294833,-2.02349677980574,0.87544890298952));
#13665=CARTESIAN_POINT('Ctrl Pts',(92.3699100774418,-1.99988529071204,0.928111369000052));
#13666=CARTESIAN_POINT('Ctrl Pts',(92.3667719254002,-1.97428890545549,0.979693481551935));
#13667=CARTESIAN_POINT('Ctrl Pts',(92.3626988604202,-1.94106688847823,1.04664284966569));
#13668=CARTESIAN_POINT('Ctrl Pts',(92.3586257954403,-1.90437150272862,1.11202954067353));
#13669=CARTESIAN_POINT('Ctrl Pts',(92.3545527304603,-1.86437310865938,1.17546965580051));
#13670=CARTESIAN_POINT('Ctrl Pts',(92.3504856496126,-1.82443348008519,1.23881656494114));
#13671=CARTESIAN_POINT('Ctrl Pts',(92.3464185687648,-1.78120073044798,1.30022217574047));
#13672=CARTESIAN_POINT('Ctrl Pts',(92.3423514879171,-1.73489179514915,1.35932573694614));
#13673=CARTESIAN_POINT('Ctrl Pts',(92.3382891655078,-1.68863704077807,1.41836014765723));
#13674=CARTESIAN_POINT('Ctrl Pts',(92.3342268430984,-1.63931354433605,1.47509748594237));
#13675=CARTESIAN_POINT('Ctrl Pts',(92.330164520689,-1.58718144445485,1.52920602352274));
#13676=CARTESIAN_POINT('Ctrl Pts',(92.3261047765105,-1.53508243121155,1.58328022008108));
#13677=CARTESIAN_POINT('Ctrl Pts',(92.3220450323321,-1.48017868221333,1.6347285837659));
#13678=CARTESIAN_POINT('Ctrl Pts',(92.3179852881536,-1.42276962835954,1.68325357109904));
#13679=CARTESIAN_POINT('Ctrl Pts',(92.3139268086607,-1.36537845849114,1.73176344199833));
#13680=CARTESIAN_POINT('Ctrl Pts',(92.3098683291679,-1.30548389772671,1.77735143665518));
#13681=CARTESIAN_POINT('Ctrl Pts',(92.3058098496751,-1.24341994265218,1.81975900773011));
#13682=CARTESIAN_POINT('Ctrl Pts',(92.3017513230063,-1.18135526614401,1.86216707175215));
#13683=CARTESIAN_POINT('Ctrl Pts',(92.2976927963376,-1.11712154048893,1.90139437090195));
#13684=CARTESIAN_POINT('Ctrl Pts',(92.2936342696688,-1.05108200374273,1.93722549575628));
#13685=CARTESIAN_POINT('Ctrl Pts',(92.2895715926498,-0.984974933324328,
1.97309326240975));
#13686=CARTESIAN_POINT('Ctrl Pts',(92.2855089156307,-0.917058784726257,
2.00555769115483));
#13687=CARTESIAN_POINT('Ctrl Pts',(92.2814462386117,-0.84772101607827,2.03444957639634));
#13688=CARTESIAN_POINT('Ctrl Pts',(92.277381439602,-0.77834703138449,2.0633565522567));
#13689=CARTESIAN_POINT('Ctrl Pts',(92.2733166405923,-0.707550397932581,
2.0886871076851));
#13690=CARTESIAN_POINT('Ctrl Pts',(92.2692518415826,-0.635735642741988,
2.11032134817128));
#13691=CARTESIAN_POINT('Ctrl Pts',(92.2651797813105,-0.5637925993416,2.13199423556191));
#13692=CARTESIAN_POINT('Ctrl Pts',(92.2611077210383,-0.490828265697908,
2.14995750469995));
#13693=CARTESIAN_POINT('Ctrl Pts',(92.2570356607661,-0.417258872264442,
2.16414210104526));
#13694=CARTESIAN_POINT('Ctrl Pts',(92.2538975103044,-0.360562308231048,
2.17507352017824));
#13695=CARTESIAN_POINT('Ctrl Pts',(92.2507593598427,-0.303506649324913,
2.18376180015199));
#13696=CARTESIAN_POINT('Ctrl Pts',(92.247621209381,-0.246283563827301,2.19019643095968));
#13697=CARTESIAN_POINT('Ctrl Pts',(92.2431657553906,-0.165039905266901,
2.19933213106666));
#13698=CARTESIAN_POINT('Ctrl Pts',(92.2387103014003,-0.0832786634272042,
2.20394849620317));
#13699=CARTESIAN_POINT('Ctrl Pts',(92.23425484741,-0.00137440780056379,
2.20399957146166));
#13700=CARTESIAN_POINT('',(91.4842548474582,-0.0010753174540008,2.20399973767974));
#13701=CARTESIAN_POINT('Ctrl Pts',(92.2342548473559,-0.0013744068059098,
2.20399957146228));
#13702=CARTESIAN_POINT('Ctrl Pts',(92.2302387400664,0.0724533734342382,
2.20404561022061));
#13703=CARTESIAN_POINT('Ctrl Pts',(92.2262226327769,0.146428553931805,2.20037789196652));
#13704=CARTESIAN_POINT('Ctrl Pts',(92.2222065254874,0.220140399541928,2.19297838669001));
#13705=CARTESIAN_POINT('Ctrl Pts',(92.2181961246188,0.293747509200828,2.18558939524906));
#13706=CARTESIAN_POINT('Ctrl Pts',(92.2141857237502,0.367091541643953,2.17447919365826));
#13707=CARTESIAN_POINT('Ctrl Pts',(92.2101753228816,0.439762030251839,2.1596817721018));
#13708=CARTESIAN_POINT('Ctrl Pts',(92.2061680589867,0.512375675311427,2.14489592522941));
#13709=CARTESIAN_POINT('Ctrl Pts',(92.2021607950919,0.584316341462203,2.12642867372763));
#13710=CARTESIAN_POINT('Ctrl Pts',(92.1981535311971,0.655180387247884,2.10436561941259));
#13711=CARTESIAN_POINT('Ctrl Pts',(92.1941480252822,0.726013345094562,2.08231224412277));
#13712=CARTESIAN_POINT('Ctrl Pts',(92.1901425193674,0.795770150846152,2.05666634077465));
#13713=CARTESIAN_POINT('Ctrl Pts',(92.1861370134526,0.864060794999802,2.02756379493823));
#13714=CARTESIAN_POINT('Ctrl Pts',(92.1821318889681,0.932344936073281,1.99846402043588));
#13715=CARTESIAN_POINT('Ctrl Pts',(92.1781267644837,0.999162741319519,1.96590845093099));
#13716=CARTESIAN_POINT('Ctrl Pts',(92.1741216399992,1.064144396598,1.93008100948874));
#13717=CARTESIAN_POINT('Ctrl Pts',(92.1701128062925,1.12918623262785,1.89422038756907));
#13718=CARTESIAN_POINT('Ctrl Pts',(92.1661039725858,1.19238809133431,1.85508207992179));
#13719=CARTESIAN_POINT('Ctrl Pts',(92.1620951388791,1.2534058599113,1.81289540523992));
#13720=CARTESIAN_POINT('Ctrl Pts',(92.1580844473776,1.31445190566342,1.77068918018746));
#13721=CARTESIAN_POINT('Ctrl Pts',(92.1540737558761,1.37331145722272,1.72543207662454));
#13722=CARTESIAN_POINT('Ctrl Pts',(92.1500630643746,1.42967270748152,1.67739439294475));
#13723=CARTESIAN_POINT('Ctrl Pts',(92.1460452816161,1.48613360941294,1.62927177439382));
#13724=CARTESIAN_POINT('Ctrl Pts',(92.1420274988575,1.54008703202777,1.57835909641725));
#13725=CARTESIAN_POINT('Ctrl Pts',(92.1380097160989,1.59125779570186,1.52496381190442));
#13726=CARTESIAN_POINT('Ctrl Pts',(92.1348299751866,1.63175519950507,1.48270588486085));
#13727=CARTESIAN_POINT('Ctrl Pts',(92.1316502342742,1.670510419511,1.43889377606131));
#13728=CARTESIAN_POINT('Ctrl Pts',(92.1284704933619,1.70740591897501,1.3936933048017));
#13729=CARTESIAN_POINT('Ctrl Pts',(92.124397429607,1.75466691467617,1.33579412173266));
#13730=CARTESIAN_POINT('Ctrl Pts',(92.120324365852,1.79907061672403,1.27537658465011));
#13731=CARTESIAN_POINT('Ctrl Pts',(92.1162513020971,1.84033770764652,1.212754353451));
#13732=CARTESIAN_POINT('Ctrl Pts',(92.112184222473,1.8815441691054,1.15022412661185));
#13733=CARTESIAN_POINT('Ctrl Pts',(92.1081171428489,1.91962290824784,1.08549603201815));
#13734=CARTESIAN_POINT('Ctrl Pts',(92.1040500632247,1.95433491919863,1.01891659305406));
#13735=CARTESIAN_POINT('Ctrl Pts',(92.0999877420311,1.98900631754633,0.952415051170976));
#13736=CARTESIAN_POINT('Ctrl Pts',(92.0959254208374,2.02031859402991,0.884066889609817));
#13737=CARTESIAN_POINT('Ctrl Pts',(92.0918630996438,2.04807701364881,0.814245998555335));
#13738=CARTESIAN_POINT('Ctrl Pts',(92.0878033566756,2.07581781588542,0.744469420590216));
#13739=CARTESIAN_POINT('Ctrl Pts',(92.0837436137075,2.10000906114561,0.673222410490049));
#13740=CARTESIAN_POINT('Ctrl Pts',(92.0796838707393,2.12050337198444,0.600900532037216));
#13741=CARTESIAN_POINT('Ctrl Pts',(92.0756253924497,2.14099129849895,0.528601183072256));
#13742=CARTESIAN_POINT('Ctrl Pts',(92.0715669141601,2.15778444706843,0.455228089637544));
#13743=CARTESIAN_POINT('Ctrl Pts',(92.0675084358706,2.17078522852257,0.381192197753571));
#13744=CARTESIAN_POINT('Ctrl Pts',(92.0634499103963,2.18378616112626,0.307155445114334));
#13745=CARTESIAN_POINT('Ctrl Pts',(92.0593913849222,2.19299455825756,0.232456349301329));
#13746=CARTESIAN_POINT('Ctrl Pts',(92.0553328594479,2.19836419316657,0.157514679325787));
#13747=CARTESIAN_POINT('Ctrl Pts',(92.0512701836017,2.20373931922807,0.082496371711897));
#13748=CARTESIAN_POINT('Ctrl Pts',(92.0472075077555,2.20526780959875,0.00723547186445174));
#13749=CARTESIAN_POINT('Ctrl Pts',(92.0431448319093,2.2029555192246,-0.0678452674684539));
#13750=CARTESIAN_POINT('Ctrl Pts',(92.0390800340623,2.20064202110406,-0.142965222677246));
#13751=CARTESIAN_POINT('Ctrl Pts',(92.0350152362152,2.19448378642386,-0.217904353679332));
#13752=CARTESIAN_POINT('Ctrl Pts',(92.0309504383682,2.18453862945074,-0.292244720119107));
#13753=CARTESIAN_POINT('Ctrl Pts',(92.0268783792288,2.17457570660222,-0.366717887045642));
#13754=CARTESIAN_POINT('Ctrl Pts',(92.0228063200895,2.16081243668112,-0.4405896828391));
#13755=CARTESIAN_POINT('Ctrl Pts',(92.0187342609501,2.14335777058606,-0.513452497577281));
#13756=CARTESIAN_POINT('Ctrl Pts',(92.0155960997477,2.12990620859569,-0.569604741562107));
#13757=CARTESIAN_POINT('Ctrl Pts',(92.0124579385452,2.11426333756261,-0.625157938330927));
#13758=CARTESIAN_POINT('Ctrl Pts',(92.0093197773427,2.09649871821207,-0.67993317652188));
#13759=CARTESIAN_POINT('Ctrl Pts',(92.0052467117079,2.07344175716888,-0.751026764748001));
#13760=CARTESIAN_POINT('Ctrl Pts',(92.001173646073,2.04671999095601,-0.821083308681164));
#13761=CARTESIAN_POINT('Ctrl Pts',(91.9971005804382,2.01644570916557,-0.889698095978488));
#13762=CARTESIAN_POINT('Ctrl Pts',(91.993033498944,1.98621590629478,-0.958212074555331));
#13763=CARTESIAN_POINT('Ctrl Pts',(91.9889664174498,1.95244414152328,-1.02528806883605));
#13764=CARTESIAN_POINT('Ctrl Pts',(91.9848993359555,1.91529216765947,-1.0905374420451));
#13765=CARTESIAN_POINT('Ctrl Pts',(91.980837012915,1.8781836613162,-1.15571047399486));
#13766=CARTESIAN_POINT('Ctrl Pts',(91.9767746898745,1.83770303826206,-1.21906071803572));
#13767=CARTESIAN_POINT('Ctrl Pts',(91.972712366834,1.79405903980528,-1.2802219189238));
#13768=CARTESIAN_POINT('Ctrl Pts',(91.9686526220341,1.75044274094981,-1.34134430254171));
#13769=CARTESIAN_POINT('Ctrl Pts',(91.9645928772342,1.70366732739993,-1.40028001230021));
#13770=CARTESIAN_POINT('Ctrl Pts',(91.9605331324343,1.65398541629023,-1.45669085350984));
#13771=CARTESIAN_POINT('Ctrl Pts',(91.9564746523305,1.60431898214355,-1.51308412155283));
#13772=CARTESIAN_POINT('Ctrl Pts',(91.9524161722267,1.55174816350242,-1.56695372463285));
#13773=CARTESIAN_POINT('Ctrl Pts',(91.948357692123,1.49656548249368,-1.61799498040274));
#13774=CARTESIAN_POINT('Ctrl Pts',(91.9442991648546,1.441382160193,-1.66903682933602));
#13775=CARTESIAN_POINT('Ctrl Pts',(91.9402406375861,1.38358726698711,-1.71724994280651));
#13776=CARTESIAN_POINT('Ctrl Pts',(91.9361821103177,1.32350856989508,-1.76236802780074));
#13777=CARTESIAN_POINT('Ctrl Pts',(91.9321194327205,1.26336843516074,-1.80753225142484));
#13778=CARTESIAN_POINT('Ctrl Pts',(91.9280567551233,1.20094021539189,-1.8495948388225));
#13779=CARTESIAN_POINT('Ctrl Pts',(91.9239940775261,1.13658240435961,-1.8883316546889));
#13780=CARTESIAN_POINT('Ctrl Pts',(91.9199292779492,1.07219097855911,-1.92708870320564));
#13781=CARTESIAN_POINT('Ctrl Pts',(91.9158644783724,1.00586837600202,-1.96251629578272));
#13782=CARTESIAN_POINT('Ctrl Pts',(91.9117996787955,0.937997198317188,-1.99443657606581));
#13783=CARTESIAN_POINT('Ctrl Pts',(91.9077276179805,0.870004777560957,-2.02641387779678));
#13784=CARTESIAN_POINT('Ctrl Pts',(91.9036555571654,0.800458698702858,-2.0548711715784));
#13785=CARTESIAN_POINT('Ctrl Pts',(91.8995834963504,0.729760587596923,-2.07967917833261));
#13786=CARTESIAN_POINT('Ctrl Pts',(91.8964453513415,0.675276891359718,-2.09879753783477));
#13787=CARTESIAN_POINT('Ctrl Pts',(91.8933072063326,0.620109401788552,-2.1157495609114));
#13788=CARTESIAN_POINT('Ctrl Pts',(91.8901690613237,0.564446179252859,-2.13049677557298));
#13789=CARTESIAN_POINT('Ctrl Pts',(91.8860959932116,0.492199646322581,-2.14963751304994));
#13790=CARTESIAN_POINT('Ctrl Pts',(91.8820229250996,0.418839076505349,-2.16513610574375));
#13791=CARTESIAN_POINT('Ctrl Pts',(91.8779498569875,0.344765469576315,-2.17686765123372));
#13792=CARTESIAN_POINT('Ctrl Pts',(91.8738827729859,0.270800690841802,-2.18858196085565));
#13793=CARTESIAN_POINT('Ctrl Pts',(91.8698156889843,0.196125422550429,-2.19654013746261));
#13794=CARTESIAN_POINT('Ctrl Pts',(91.8657486049827,0.121153953181855,-2.20066756227023));
#13795=CARTESIAN_POINT('Ctrl Pts',(91.8616862794022,0.0462701991927912,
-2.20479015805908));
#13796=CARTESIAN_POINT('Ctrl Pts',(91.8576239538217,-0.0289085930146785,
-2.20509088047959));
#13797=CARTESIAN_POINT('Ctrl Pts',(91.8535616282411,-0.103961487225625,
-2.20154673109018));
#13798=CARTESIAN_POINT('Ctrl Pts',(91.8495018808824,-0.178966747880666,
-2.19800483105357));
#13799=CARTESIAN_POINT('Ctrl Pts',(91.8454421335237,-0.253845793378832,
-2.19062292400726));
#13800=CARTESIAN_POINT('Ctrl Pts',(91.8413823861651,-0.328177499460303,
-2.17943009267285));
#13801=CARTESIAN_POINT('Ctrl Pts',(91.8373239034875,-0.402486049936229,
-2.168240748098));
#13802=CARTESIAN_POINT('Ctrl Pts',(91.83326542081,-0.47624712769799,-2.15324290735523));
#13803=CARTESIAN_POINT('Ctrl Pts',(91.8292069381325,-0.54904615410687,-2.13451735075179));
#13804=CARTESIAN_POINT('Ctrl Pts',(91.8251484082791,-0.621846026731769,
-2.11579157648245));
#13805=CARTESIAN_POINT('Ctrl Pts',(91.8210898784258,-0.693683363838802,
-2.09333812099535));
#13806=CARTESIAN_POINT('Ctrl Pts',(91.8170313485725,-0.764156756421241,
-2.06728818784798));
#13807=CARTESIAN_POINT('Ctrl Pts',(91.8129686683913,-0.834702216401371,
-2.04121161555605));
#13808=CARTESIAN_POINT('Ctrl Pts',(91.8089059882101,-0.903880497692544,
-2.01153138710734));
#13809=CARTESIAN_POINT('Ctrl Pts',(91.8048433080289,-0.971308976230853,
-1.97842737362112));
#13810=CARTESIAN_POINT('Ctrl Pts',(91.8007785058645,-1.03877267341609,-1.94530606953918));
#13811=CARTESIAN_POINT('Ctrl Pts',(91.7967137037001,-1.1044843301727,-1.9087576515262));
#13812=CARTESIAN_POINT('Ctrl Pts',(91.7926489015357,-1.16808715750088,-1.86900732809733));
#13813=CARTESIAN_POINT('Ctrl Pts',(91.788576838157,-1.23180360259935,-1.82918599614092));
#13814=CARTESIAN_POINT('Ctrl Pts',(91.7845047747783,-1.2934033017218,-1.78615160782476));
#13815=CARTESIAN_POINT('Ctrl Pts',(91.7804327113996,-1.35255998707582,-1.74017168157669));
#13816=CARTESIAN_POINT('Ctrl Pts',(91.7772945893679,-1.3981488889097,-1.70473740510383));
#13817=CARTESIAN_POINT('Ctrl Pts',(91.7741564673362,-1.44228751156915,-1.66755466486185));
#13818=CARTESIAN_POINT('Ctrl Pts',(91.7710183453045,-1.48484162758654,-1.62876067639975));
#13819=CARTESIAN_POINT('Ctrl Pts',(91.7669452899945,-1.54007379078977,-1.57840888666531));
#13820=CARTESIAN_POINT('Ctrl Pts',(91.7628722346845,-1.59284838009649,-1.52514738068764));
#13821=CARTESIAN_POINT('Ctrl Pts',(91.7587991793745,-1.64284314659156,-1.46924551920268));
#13822=CARTESIAN_POINT('Ctrl Pts',(91.7547321082011,-1.69276446072964,-1.41342578878411));
#13823=CARTESIAN_POINT('Ctrl Pts',(91.7506650370278,-1.73991374504865,-1.35497375761978));
#13824=CARTESIAN_POINT('Ctrl Pts',(91.7465979658544,-1.78400381349604,-1.29419720036461));
#13825=CARTESIAN_POINT('Ctrl Pts',(91.7425356530804,-1.82804229736444,-1.23349175057714));
#13826=CARTESIAN_POINT('Ctrl Pts',(91.7384733403064,-1.86902839750786,-1.17046756256348));
#13827=CARTESIAN_POINT('Ctrl Pts',(91.7344110275324,-1.90671471248638,-1.10546596744901));
#13828=CARTESIAN_POINT('Ctrl Pts',(91.7303512929608,-1.944377109329,-1.04050562648706));
#13829=CARTESIAN_POINT('Ctrl Pts',(91.7262915583892,-1.97874363795094,-0.973570780826892));
#13830=CARTESIAN_POINT('Ctrl Pts',(91.7222318238177,-2.00961056888026,-0.905031138384061));
#13831=CARTESIAN_POINT('Ctrl Pts',(91.7181733538899,-2.0404678844829,-0.8365128466565));
#13832=CARTESIAN_POINT('Ctrl Pts',(91.7141148839622,-2.06782757091763,-0.766391185760943));
#13833=CARTESIAN_POINT('Ctrl Pts',(91.7100564140345,-2.09153289675691,-0.695058372932542));
#13834=CARTESIAN_POINT('Ctrl Pts',(91.7059978968757,-2.11523849847037,-0.623724729958193));
#13835=CARTESIAN_POINT('Ctrl Pts',(91.701939379717,-2.13528950627479,-0.551180360729292));
#13836=CARTESIAN_POINT('Ctrl Pts',(91.6978808625582,-2.15157870476266,-0.477833733857121));
#13837=CARTESIAN_POINT('Ctrl Pts',(91.6938181948983,-2.16788456163447,-0.404412097998338));
#13838=CARTESIAN_POINT('Ctrl Pts',(91.6897555272384,-2.18042082306836,-0.330187033266231));
#13839=CARTESIAN_POINT('Ctrl Pts',(91.6856928595785,-2.18913135652916,-0.255577588729571));
#13840=CARTESIAN_POINT('Ctrl Pts',(91.681628069859,-2.19784643977656,-0.180929173324751));
#13841=CARTESIAN_POINT('Ctrl Pts',(91.6775632801395,-2.20273178458476,-0.105896455191822));
#13842=CARTESIAN_POINT('Ctrl Pts',(91.6734984904201,-2.20378336221302,-0.0309013338396533));
#13843=CARTESIAN_POINT('Ctrl Pts',(91.6694264392199,-2.20483681841586,0.0442277613854869));
#13844=CARTESIAN_POINT('Ctrl Pts',(91.6653543880198,-2.20204284532493,0.119318647833614));
#13845=CARTESIAN_POINT('Ctrl Pts',(91.6612823368197,-2.19544951245386,0.193952154579663));
#13846=CARTESIAN_POINT('Ctrl Pts',(91.658144100975,-2.19036818303649,0.251470475096262));
#13847=CARTESIAN_POINT('Ctrl Pts',(91.6550058651302,-2.18303132525941,0.308717180314805));
#13848=CARTESIAN_POINT('Ctrl Pts',(91.6518676292855,-2.1734815463362,0.365505085786788));
#13849=CARTESIAN_POINT('Ctrl Pts',(91.6477945561724,-2.16108701970002,0.43920932675874));
#13850=CARTESIAN_POINT('Ctrl Pts',(91.6437214830593,-2.14491530015174,0.512424525006328));
#13851=CARTESIAN_POINT('Ctrl Pts',(91.6396484099462,-2.12501818452048,0.584733884307464));
#13852=CARTESIAN_POINT('Ctrl Pts',(91.6355813210328,-2.10515030193009,0.656937005976228));
#13853=CARTESIAN_POINT('Ctrl Pts',(91.6315142321194,-2.08156801578952,0.728236474486894));
#13854=CARTESIAN_POINT('Ctrl Pts',(91.6274471432059,-2.054374407353,0.798224150482185));
#13855=CARTESIAN_POINT('Ctrl Pts',(91.6233848128683,-2.02721261598494,0.868129939489815));
#13856=CARTESIAN_POINT('Ctrl Pts',(91.6193224825306,-1.9964480691207,0.936726542518279));
#13857=CARTESIAN_POINT('Ctrl Pts',(91.615260152193,-1.96223360810615,1.0036210775082));
#13858=CARTESIAN_POINT('Ctrl Pts',(91.611200400174,-1.92804086265294,1.07047315523488));
#13859=CARTESIAN_POINT('Ctrl Pts',(91.607140648155,-1.89040276498942,1.13562488462496));
#13860=CARTESIAN_POINT('Ctrl Pts',(91.603080896136,-1.84951966932641,1.19870471458768));
#13861=CARTESIAN_POINT('Ctrl Pts',(91.5990224089008,-1.80864931046897,1.26176489252755));
#13862=CARTESIAN_POINT('Ctrl Pts',(91.5949639216654,-1.76453622032653,1.32275405221568));
#13863=CARTESIAN_POINT('Ctrl Pts',(91.5909054344301,-1.71742513656064,1.38132794813891));
#13864=CARTESIAN_POINT('Ctrl Pts',(91.5868469001273,-1.67031350643343,1.43990252336113));
#13865=CARTESIAN_POINT('Ctrl Pts',(91.5827883658245,-1.62020411428653,1.49606140827559));
#13866=CARTESIAN_POINT('Ctrl Pts',(91.5787298315217,-1.5673821857963,1.54949316992636));
#13867=CARTESIAN_POINT('Ctrl Pts',(91.5746671470881,-1.514506243246,1.6029795692336));
#13868=CARTESIAN_POINT('Ctrl Pts',(91.5706044626544,-1.45891256173779,1.65373293615841));
#13869=CARTESIAN_POINT('Ctrl Pts',(91.5665417782208,-1.40092293754828,1.70147903985065));
#13870=CARTESIAN_POINT('Ctrl Pts',(91.5624769719064,-1.34290302622578,1.74925008063488));
#13871=CARTESIAN_POINT('Ctrl Pts',(91.5584121655921,-1.28248506425117,1.79401044590272));
#13872=CARTESIAN_POINT('Ctrl Pts',(91.5543473592777,-1.22002147472927,1.83552815320262));
#13873=CARTESIAN_POINT('Ctrl Pts',(91.5502752919629,-1.15744630592912,1.87712002396079));
#13874=CARTESIAN_POINT('Ctrl Pts',(91.5462032246481,-1.09281862200705,1.9154574229452));
#13875=CARTESIAN_POINT('Ctrl Pts',(91.5421311573332,-1.0265167807496,1.95035363430314));
#13876=CARTESIAN_POINT('Ctrl Pts',(91.5389930759776,-0.975422200083803,
1.97724590836889));
#13877=CARTESIAN_POINT('Ctrl Pts',(91.5358549946219,-0.923333918039295,
2.00209545679016));
#13878=CARTESIAN_POINT('Ctrl Pts',(91.5327169132663,-0.870432319660632,
2.0248366790658));
#13879=CARTESIAN_POINT('Ctrl Pts',(91.5282130966559,-0.794507233441178,
2.0574751874461));
#13880=CARTESIAN_POINT('Ctrl Pts',(91.5237092800456,-0.716656622068216,
2.0858771805404));
#13881=CARTESIAN_POINT('Ctrl Pts',(91.5192054634353,-0.637345146763546,
2.10983581444077));
#13882=CARTESIAN_POINT('Ctrl Pts',(91.5147154542498,-0.558276817957318,
2.13372099796189));
#13883=CARTESIAN_POINT('Ctrl Pts',(91.5102254450644,-0.477756831322773,
2.15318986501427));
#13884=CARTESIAN_POINT('Ctrl Pts',(91.505735435879,-0.396268453458691,2.16808378823178));
#13885=CARTESIAN_POINT('Ctrl Pts',(91.5012685484843,-0.315199708861933,
2.1829010135713));
#13886=CARTESIAN_POINT('Ctrl Pts',(91.4968016610897,-0.233172802184434,
2.19319016597525));
#13887=CARTESIAN_POINT('Ctrl Pts',(91.492334773695,-0.150682170051668,2.19884307844569));
#13888=CARTESIAN_POINT('Ctrl Pts',(91.4896414649494,-0.100944462040351,
2.20225150074286));
#13889=CARTESIAN_POINT('Ctrl Pts',(91.4869481562038,-0.0510385083173603,
2.2039753609567));
#13890=CARTESIAN_POINT('Ctrl Pts',(91.4842548474582,-0.0010753174540001,
2.20399973767974));
#13891=CARTESIAN_POINT('',(90.7342548473723,0.00189326485402309,2.2039991868302));
#13892=CARTESIAN_POINT('Ctrl Pts',(91.48425484741,-0.00107531656039788,
2.20399973768018));
#13893=CARTESIAN_POINT('Ctrl Pts',(91.4801345475516,0.0753597852745452,
2.20403702984923));
#13894=CARTESIAN_POINT('Ctrl Pts',(91.4760142476932,0.151787090692672,2.20009380347946));
#13895=CARTESIAN_POINT('Ctrl Pts',(91.4718939478347,0.22777218684923,2.19219885751679));
#13896=CARTESIAN_POINT('Ctrl Pts',(91.4677719624903,0.303788366135591,2.18430068197829));
#13897=CARTESIAN_POINT('Ctrl Pts',(91.4636499771459,0.379361522226958,2.17244762155421));
#13898=CARTESIAN_POINT('Ctrl Pts',(91.4595279918015,0.45406412797954,2.15672014125203));
#13899=CARTESIAN_POINT('Ctrl Pts',(91.4553998074611,0.528879077931765,2.14096900861311));
#13900=CARTESIAN_POINT('Ctrl Pts',(91.4512716231209,0.60282041544042,2.12133191698089));
#13901=CARTESIAN_POINT('Ctrl Pts',(91.4471434387806,0.675472845712013,2.09794004554604));
#13902=CARTESIAN_POINT('Ctrl Pts',(91.4430119747139,0.74818299629565,2.07452958992737));
#13903=CARTESIAN_POINT('Ctrl Pts',(91.4388805106473,0.819601773231825,2.04735857617575));
#13904=CARTESIAN_POINT('Ctrl Pts',(91.4347490465807,0.889333527039305,2.01660652525073));
#13905=CARTESIAN_POINT('Ctrl Pts',(91.4306090428813,0.959209414635745,1.98579091060651));
#13906=CARTESIAN_POINT('Ctrl Pts',(91.4264690391819,1.02739090475845,1.95137967828839));
#13907=CARTESIAN_POINT('Ctrl Pts',(91.4223290354825,1.09350671021836,1.91359846224526));
#13908=CARTESIAN_POINT('Ctrl Pts',(91.419408089404,1.14015418126097,1.88694223127194));
#13909=CARTESIAN_POINT('Ctrl Pts',(91.4164871433255,1.18577393310765,1.85860941038486));
#13910=CARTESIAN_POINT('Ctrl Pts',(91.4135661972471,1.23024510906643,1.82869160101372));
#13911=CARTESIAN_POINT('Ctrl Pts',(91.4094932090485,1.292256036344,1.78697399267035));
#13912=CARTESIAN_POINT('Ctrl Pts',(91.40542022085,1.3522622016404,1.74201815661329));
#13913=CARTESIAN_POINT('Ctrl Pts',(91.4013472326515,1.40990538202678,1.69404333289675));
#13914=CARTESIAN_POINT('Ctrl Pts',(91.3972802286801,1.46746387032373,1.64613899606233));
#13915=CARTESIAN_POINT('Ctrl Pts',(91.3932132247086,1.52266590270625,1.59522478102214));
#13916=CARTESIAN_POINT('Ctrl Pts',(91.3891462207372,1.57518231321275,1.54156306395222));
#13917=CARTESIAN_POINT('Ctrl Pts',(91.3850839749833,1.62763728180575,1.48796412875459));
#13918=CARTESIAN_POINT('Ctrl Pts',(91.3810217292294,1.67741253878216,1.4316244174492));
#13919=CARTESIAN_POINT('Ctrl Pts',(91.3769594834755,1.72421335770118,1.3728453289154));
#13920=CARTESIAN_POINT('Ctrl Pts',(91.3728998157806,1.7709844750023,1.31410354387476));
#13921=CARTESIAN_POINT('Ctrl Pts',(91.3688401480857,1.81478460350243,1.25292582627685));
#13922=CARTESIAN_POINT('Ctrl Pts',(91.3647804803908,1.85535806068537,1.18964804318329));
#13923=CARTESIAN_POINT('Ctrl Pts',(91.3607220771031,1.89591888102782,1.12638996832528));
#13924=CARTESIAN_POINT('Ctrl Pts',(91.3566636738155,1.93325476780625,1.06103352830072));
#13925=CARTESIAN_POINT('Ctrl Pts',(91.3526052705278,1.96715323228298,0.993943741224126));
#13926=CARTESIAN_POINT('Ctrl Pts',(91.3485468196791,2.0010520940205,0.926853167913054));
#13927=CARTESIAN_POINT('Ctrl Pts',(91.3444883688305,2.03151323974132,0.858029634195111));
#13928=CARTESIAN_POINT('Ctrl Pts',(91.3404299179818,2.05837078210288,0.7878614874362));
#13929=CARTESIAN_POINT('Ctrl Pts',(91.3363673156635,2.08525579757623,0.717621564290818));
#13930=CARTESIAN_POINT('Ctrl Pts',(91.3323047133451,2.10852967750412,0.646034728369659));
#13931=CARTESIAN_POINT('Ctrl Pts',(91.3282421110267,2.12807551660858,0.573507275987955));
#13932=CARTESIAN_POINT('Ctrl Pts',(91.3241773862146,2.14763156737461,0.500941931869087));
#13933=CARTESIAN_POINT('Ctrl Pts',(91.3201126614026,2.16345559808519,0.427435459893576));
#13934=CARTESIAN_POINT('Ctrl Pts',(91.3160479365905,2.17548182781943,0.353404607818623));
#13935=CARTESIAN_POINT('Ctrl Pts',(91.3119759488505,2.18752954625082,0.279241476002225));
#13936=CARTESIAN_POINT('Ctrl Pts',(91.3079039611105,2.19576585682346,0.204552567865129));
#13937=CARTESIAN_POINT('Ctrl Pts',(91.3038319733704,2.20017691466317,0.129759562974175));
#13938=CARTESIAN_POINT('Ctrl Pts',(91.3006931426563,2.2035771124813,0.0721064962309344));
#13939=CARTESIAN_POINT('Ctrl Pts',(91.2975543119422,2.20470546515236,0.0143916924216315));
#13940=CARTESIAN_POINT('Ctrl Pts',(91.294415481228,2.20357671439982,-0.0431933299815596));
#13941=CARTESIAN_POINT('Ctrl Pts',(91.2903423321053,2.20211197464282,-0.117919368065657));
#13942=CARTESIAN_POINT('Ctrl Pts',(91.2862691829825,2.19683902233028,-0.192714898337843));
#13943=CARTESIAN_POINT('Ctrl Pts',(91.2821960338598,2.18774804839455,-0.267160020859897));
#13944=CARTESIAN_POINT('Ctrl Pts',(91.2781288693383,2.17867043165546,-0.341495762566669));
#13945=CARTESIAN_POINT('Ctrl Pts',(91.2740617048168,2.16578598833572,-0.415481648720905));
#13946=CARTESIAN_POINT('Ctrl Pts',(91.2699945402953,2.14913690866279,-0.488698831411888));
#13947=CARTESIAN_POINT('Ctrl Pts',(91.2659321352976,2.13250731226656,-0.561830333052806));
#13948=CARTESIAN_POINT('Ctrl Pts',(91.2618697303,2.11212193757829,-0.63419445523976));
#13949=CARTESIAN_POINT('Ctrl Pts',(91.2578073253023,2.08807443297473,-0.705380154496332));
#13950=CARTESIAN_POINT('Ctrl Pts',(91.2537474992385,2.0640421944325,-0.776520662982861));
#13951=CARTESIAN_POINT('Ctrl Pts',(91.2496876731747,2.03635259176569,-0.846483781878596));
#13952=CARTESIAN_POINT('Ctrl Pts',(91.2456278471109,2.00514939821203,-0.914872609082792));
#13953=CARTESIAN_POINT('Ctrl Pts',(91.2415692865451,1.97395593107933,-0.983240118644564));
#13954=CARTESIAN_POINT('Ctrl Pts',(91.2375107259792,1.93925124564859,-1.05003387675144));
#13955=CARTESIAN_POINT('Ctrl Pts',(91.2334521654133,1.90122701960133,-1.11487749099972));
#13956=CARTESIAN_POINT('Ctrl Pts',(91.229393558594,1.86320236021025,-1.1797218442395));
#13957=CARTESIAN_POINT('Ctrl Pts',(91.2253349517747,1.82185832814373,-1.24261559854748));
#13958=CARTESIAN_POINT('Ctrl Pts',(91.2212763449554,1.77743145891488,-1.30320888918842));
#13959=CARTESIAN_POINT('Ctrl Pts',(91.2172135897585,1.73295918015641,-1.3638641133591));
#13960=CARTESIAN_POINT('Ctrl Pts',(91.2131508345617,1.68539805474719,-1.42221379246401));
#13961=CARTESIAN_POINT('Ctrl Pts',(91.2090880793648,1.6350262438774,-1.4779395054711));
#13962=CARTESIAN_POINT('Ctrl Pts',(91.205023203148,1.58462813567742,-1.5336943108902));
#13963=CARTESIAN_POINT('Ctrl Pts',(91.2009583269312,1.53141675808621,-1.58682208457118));
#13964=CARTESIAN_POINT('Ctrl Pts',(91.1968934507144,1.47570675792028,-1.63704171132821));
#13965=CARTESIAN_POINT('Ctrl Pts',(91.1928213156935,1.41989727428702,-1.68735101718385));
#13966=CARTESIAN_POINT('Ctrl Pts',(91.1887491806725,1.36158062687592,-1.73474150156833));
#13967=CARTESIAN_POINT('Ctrl Pts',(91.1846770456516,1.30110374867889,-1.7789730282311));
#13968=CARTESIAN_POINT('Ctrl Pts',(91.1815396188373,1.25450858954928,-1.81305175525604));
#13969=CARTESIAN_POINT('Ctrl Pts',(91.1784021920231,1.20663176737054,-1.84525612230047));
#13970=CARTESIAN_POINT('Ctrl Pts',(91.1752647652088,1.15764200097884,-1.87549486738026));
#13971=CARTESIAN_POINT('Ctrl Pts',(91.1711915775716,1.0940406733218,-1.91475254251144));
#13972=CARTESIAN_POINT('Ctrl Pts',(91.1671183899345,1.0283175516707,-1.95084696681253));
#13973=CARTESIAN_POINT('Ctrl Pts',(91.1630452022973,0.960820261995865,-1.98354239282608));
#13974=CARTESIAN_POINT('Ctrl Pts',(91.1589779973941,0.893422112936246,-2.01618979550913));
#13975=CARTESIAN_POINT('Ctrl Pts',(91.154910792491,0.824255395773518,-2.04544790562825));
#13976=CARTESIAN_POINT('Ctrl Pts',(91.1508435875878,0.753695024608214,-2.07112525209868));
#13977=CARTESIAN_POINT('Ctrl Pts',(91.1467811396405,0.683217180037177,-2.09677256664157));
#13978=CARTESIAN_POINT('Ctrl Pts',(91.1427186916931,0.611349366301141,-2.11884727574468));
#13979=CARTESIAN_POINT('Ctrl Pts',(91.1386562437458,0.53848781731309,-2.13720538802554));
#13980=CARTESIAN_POINT('Ctrl Pts',(91.1345963731848,0.465672494730524,-2.15555185315431));
#13981=CARTESIAN_POINT('Ctrl Pts',(91.1305365026239,0.391865149778248,-2.17018628424562));
#13982=CARTESIAN_POINT('Ctrl Pts',(91.126476632063,0.317477287424272,-2.18101448229252));
#13983=CARTESIAN_POINT('Ctrl Pts',(91.1224180255295,0.243112585488015,-2.19183930901537));
#13984=CARTESIAN_POINT('Ctrl Pts',(91.1183594189959,0.168168197146597,-2.19886018685535));
#13985=CARTESIAN_POINT('Ctrl Pts',(91.1143008124624,0.0930643429279588,
-2.20203429311975));
#13986=CARTESIAN_POINT('Ctrl Pts',(91.1102421582803,0.0179596069796596,
-2.2052084366486));
#13987=CARTESIAN_POINT('Ctrl Pts',(91.1061835040982,-0.0573041214864556,
-2.20453570056347));
#13988=CARTESIAN_POINT('Ctrl Pts',(91.1021248499161,-0.132304615016989,
-2.200025338228));
#13989=CARTESIAN_POINT('Ctrl Pts',(91.0980620455509,-0.207381800418263,
-2.19551036381453));
#13990=CARTESIAN_POINT('Ctrl Pts',(91.0939992411856,-0.282194735740037,
-2.1871499555293));
#13991=CARTESIAN_POINT('Ctrl Pts',(91.0899364368204,-0.356325069411539,
-2.17500538962754));
#13992=CARTESIAN_POINT('Ctrl Pts',(91.0858715103569,-0.430494123099852,
-2.16285448033338));
#13993=CARTESIAN_POINT('Ctrl Pts',(91.0818065838934,-0.50397939811163,-2.14691557859187));
#13994=CARTESIAN_POINT('Ctrl Pts',(91.0777416574299,-0.576374130845831,
-2.12730083939525));
#13995=CARTESIAN_POINT('Ctrl Pts',(91.0736694709889,-0.648898160908092,
-2.10765106818355));
#13996=CARTESIAN_POINT('Ctrl Pts',(91.0695972845479,-0.720327303794025,
-2.08431249480676));
#13997=CARTESIAN_POINT('Ctrl Pts',(91.0655250981069,-0.790271746160557,
-2.0574466134557));
#13998=CARTESIAN_POINT('Ctrl Pts',(91.0623880818012,-0.844153575830507,
-2.0367504324024));
#13999=CARTESIAN_POINT('Ctrl Pts',(91.0592510654954,-0.897154658303896,
-2.01396202043894));
#14000=CARTESIAN_POINT('Ctrl Pts',(91.0561140491897,-0.94910694297007,-1.98917370051135));
#14001=CARTESIAN_POINT('Ctrl Pts',(91.0520415827155,-1.01655126488137,-1.95699356753781));
#14002=CARTESIAN_POINT('Ctrl Pts',(91.0479691162412,-1.08248738225664,-1.92131726115899));
#14003=CARTESIAN_POINT('Ctrl Pts',(91.0438966497669,-1.14652888156507,-1.88230909357023));
#14004=CARTESIAN_POINT('Ctrl Pts',(91.0398301685679,-1.21047625953367,-1.84335825601023));
#14005=CARTESIAN_POINT('Ctrl Pts',(91.0357636873689,-1.27253414325808,-1.80108552571422));
#14006=CARTESIAN_POINT('Ctrl Pts',(91.0316972061699,-1.33233853679501,-1.7557021454025));
#14007=CARTESIAN_POINT('Ctrl Pts',(91.0276354822864,-1.39207296606744,-1.71037185842785));
#14008=CARTESIAN_POINT('Ctrl Pts',(91.0235737584028,-1.44955876432225,-1.66193843870085));
#14009=CARTESIAN_POINT('Ctrl Pts',(91.0195120345193,-1.50446028197339,-1.61065677907012));
#14010=CARTESIAN_POINT('Ctrl Pts',(91.0154528878933,-1.55932696334508,-1.55940765883543));
#14011=CARTESIAN_POINT('Ctrl Pts',(91.0113937412672,-1.61161226990499,-1.50531421019386));
#14012=CARTESIAN_POINT('Ctrl Pts',(91.0073345946412,-1.66101412244257,-1.44867114454811));
#14013=CARTESIAN_POINT('Ctrl Pts',(91.003276710894,-1.7104006051109,-1.39204570165269));
#14014=CARTESIAN_POINT('Ctrl Pts',(90.9992188271467,-1.7569051011597,-1.33287257638486));
#14015=CARTESIAN_POINT('Ctrl Pts',(90.9951609433995,-1.8002639873571,-1.27148164588606));
#14016=CARTESIAN_POINT('Ctrl Pts',(90.9911030098348,-1.84362340585925,-1.21008996170821));
#14017=CARTESIAN_POINT('Ctrl Pts',(90.9870450762701,-1.88383686376207,-1.14648080939786));
#14018=CARTESIAN_POINT('Ctrl Pts',(90.9829871427054,-1.92068341877735,-1.08101397069314));
#14019=CARTESIAN_POINT('Ctrl Pts',(90.9789250506036,-1.95756773384043,-1.0154800421083));
#14020=CARTESIAN_POINT('Ctrl Pts',(90.9748629585018,-1.99107802105361,-0.948085042622554));
#14021=CARTESIAN_POINT('Ctrl Pts',(90.9708008664,-2.02103916263345,-0.87921368455108));
#14022=CARTESIAN_POINT('Ctrl Pts',(90.9667366486916,-2.0510159822424,-0.810306287560541));
#14023=CARTESIAN_POINT('Ctrl Pts',(90.9626724309833,-2.07743978984685,-0.739921441117149));
#14024=CARTESIAN_POINT('Ctrl Pts',(90.958608213275,-2.10018451078152,-0.668461682277608));
#14025=CARTESIAN_POINT('Ctrl Pts',(90.9545367217817,-2.1229699382485,-0.596874030948583));
#14026=CARTESIAN_POINT('Ctrl Pts',(90.9504652302884,-2.14206300549317,-0.524208087245253));
#14027=CARTESIAN_POINT('Ctrl Pts',(90.9463937387951,-2.15738829210057,-0.450878871879563));
#14028=CARTESIAN_POINT('Ctrl Pts',(90.9432502702536,-2.16922045641158,-0.394263726777795));
#14029=CARTESIAN_POINT('Ctrl Pts',(90.9401068017121,-2.17880772658627,-0.337253484604036));
#14030=CARTESIAN_POINT('Ctrl Pts',(90.9369633331706,-2.18613660174063,-0.280040637283147));
#14031=CARTESIAN_POINT('Ctrl Pts',(90.932889462496,-2.1956346734329,-0.205893962093828));
#14032=CARTESIAN_POINT('Ctrl Pts',(90.9288155918213,-2.20137453506395,-0.131120765785595));
#14033=CARTESIAN_POINT('Ctrl Pts',(90.9247417211466,-2.20328501326668,-0.056135107681679));
#14034=CARTESIAN_POINT('Ctrl Pts',(90.9206738376651,-2.20519268372146,0.018740347213517));
#14035=CARTESIAN_POINT('Ctrl Pts',(90.9166059541837,-2.20328213245543,0.0938271708094514));
#14036=CARTESIAN_POINT('Ctrl Pts',(90.9125380707022,-2.19753377957874,0.168704734996868));
#14037=CARTESIAN_POINT('Ctrl Pts',(90.9084749539541,-2.19179216260434,0.243494557884093));
#14038=CARTESIAN_POINT('Ctrl Pts',(90.904411837206,-2.18222171526202,0.318075135074735));
#14039=CARTESIAN_POINT('Ctrl Pts',(90.900348720458,-2.16885490383549,0.392026027335872));
#14040=CARTESIAN_POINT('Ctrl Pts',(90.8962881873953,-2.15549659219831,0.465929895143214));
#14041=CARTESIAN_POINT('Ctrl Pts',(90.8922276543327,-2.13834679166121,0.539204404142618));
#14042=CARTESIAN_POINT('Ctrl Pts',(90.8881671212701,-2.11748962360874,0.611435764336152));
#14043=CARTESIAN_POINT('Ctrl Pts',(90.8841078594163,-2.09663898519549,0.683644511453837));
#14044=CARTESIAN_POINT('Ctrl Pts',(90.8800485975625,-2.07208341602311,0.75481029994527));
#14045=CARTESIAN_POINT('Ctrl Pts',(90.8759893357087,-2.04395742924475,0.824532611504955));
#14046=CARTESIAN_POINT('Ctrl Pts',(90.8719300342768,-2.01583116823547,0.894255602863506));
#14047=CARTESIAN_POINT('Ctrl Pts',(90.8678707328448,-1.98413460070982,0.962534647413805));
#14048=CARTESIAN_POINT('Ctrl Pts',(90.8638114314128,-1.94905050029505,1.02898889561532));
#14049=CARTESIAN_POINT('Ctrl Pts',(90.859747996683,-1.91393067623649,1.09551080945062));
#14050=CARTESIAN_POINT('Ctrl Pts',(90.8556845619531,-1.87541665453586,1.16020379348521));
#14051=CARTESIAN_POINT('Ctrl Pts',(90.8516211272232,-1.83373699234912,1.22271200324951));
#14052=CARTESIAN_POINT('Ctrl Pts',(90.847555578769,-1.79203564916534,1.28525272863988));
#14053=CARTESIAN_POINT('Ctrl Pts',(90.8434900303148,-1.7471656711554,1.34560603313343));
#14054=CARTESIAN_POINT('Ctrl Pts',(90.8394244818606,-1.69939717640751,1.4034476252494));
#14055=CARTESIAN_POINT('Ctrl Pts',(90.835351694127,-1.65154362315281,1.4613922124353));
#14056=CARTESIAN_POINT('Ctrl Pts',(90.8312789063934,-1.6007815667975,1.51681580132527));
#14057=CARTESIAN_POINT('Ctrl Pts',(90.8272061186598,-1.54741907026956,1.56942990317061));
#14058=CARTESIAN_POINT('Ctrl Pts',(90.8240749514903,-1.50639387864707,1.60987972749844));
#14059=CARTESIAN_POINT('Ctrl Pts',(90.8209437843209,-1.46383247197762,1.64866971655217));
#14060=CARTESIAN_POINT('Ctrl Pts',(90.8178126171514,-1.41988740623812,1.68568554410554));
#14061=CARTESIAN_POINT('Ctrl Pts',(90.8137657639652,-1.36309094035839,1.73352636880945));
#14062=CARTESIAN_POINT('Ctrl Pts',(90.8097189107791,-1.30375598984691,1.77859266049886));
#14063=CARTESIAN_POINT('Ctrl Pts',(90.8056720575929,-1.24218642093431,1.82060124564562));
#14064=CARTESIAN_POINT('Ctrl Pts',(90.8016308065827,-1.18070208455728,1.86255167709258));
#14065=CARTESIAN_POINT('Ctrl Pts',(90.7975895555724,-1.1169896612247,1.90145252786528));
#14066=CARTESIAN_POINT('Ctrl Pts',(90.7935483045622,-1.05138688805472,1.93706004337155));
#14067=CARTESIAN_POINT('Ctrl Pts',(90.7895113008791,-0.985853062949274,
1.97263013562332));
#14068=CARTESIAN_POINT('Ctrl Pts',(90.7854742971959,-0.918433253117161,
2.00491353132598));
#14069=CARTESIAN_POINT('Ctrl Pts',(90.7814372935128,-0.849493646490407,
2.03371004437025));
#14070=CARTESIAN_POINT('Ctrl Pts',(90.7774025713876,-0.780593001856861,
2.06249028274165));
#14071=CARTESIAN_POINT('Ctrl Pts',(90.7733678492625,-0.710174707678702,
2.08778735697564));
#14072=CARTESIAN_POINT('Ctrl Pts',(90.7693331271373,-0.638627650683483,
2.10944796659754));
#14073=CARTESIAN_POINT('Ctrl Pts',(90.7652999118247,-0.567107313745175,
2.13110048682001));
#14074=CARTESIAN_POINT('Ctrl Pts',(90.7612666965122,-0.494459514900456,
2.14911910202913));
#14075=CARTESIAN_POINT('Ctrl Pts',(90.7572334811996,-0.421089349198961,
2.1634000462215));
#14076=CARTESIAN_POINT('Ctrl Pts',(90.7531984374294,-0.347685921144087,
2.17768746467774));
#14077=CARTESIAN_POINT('Ctrl Pts',(90.7491633936593,-0.27355994683826,2.1882337298734));
#14078=CARTESIAN_POINT('Ctrl Pts',(90.7451283498892,-0.199126722959242,
2.19498622961592));
#14079=CARTESIAN_POINT('Ctrl Pts',(90.7415038490628,-0.132266659765372,
2.20105170059747));
#14080=CARTESIAN_POINT('Ctrl Pts',(90.7378793482364,-0.0651590566933283,
2.20405678565228));
#14081=CARTESIAN_POINT('Ctrl Pts',(90.73425484741,0.00189326415692431,2.2039991868308));
#14082=CARTESIAN_POINT('',(90.3498699627424,-0.173992556915814,-2.19712143272462));
#14083=CARTESIAN_POINT('Ctrl Pts',(90.7342548473723,0.00189326485402265,
2.2039991868302));
#14084=CARTESIAN_POINT('Ctrl Pts',(90.7293515116983,0.0926036971570066,
2.20392126535256));
#14085=CARTESIAN_POINT('Ctrl Pts',(90.7244481760243,0.183069156407198,2.19823945073773));
#14086=CARTESIAN_POINT('Ctrl Pts',(90.7195448403504,0.272680382344514,2.18706685062082));
#14087=CARTESIAN_POINT('Ctrl Pts',(90.7145706549739,0.363586426567747,2.17573281440277));
#14088=CARTESIAN_POINT('Ctrl Pts',(90.7095964695975,0.453613385733587,2.15874824234606));
#14089=CARTESIAN_POINT('Ctrl Pts',(90.7046222842211,0.542147312526976,2.13628001243278));
#14090=CARTESIAN_POINT('Ctrl Pts',(90.7026354898581,0.577509626829502,2.12730572837251));
#14091=CARTESIAN_POINT('Ctrl Pts',(90.7006486954952,0.612633990132352,2.1174571311083));
#14092=CARTESIAN_POINT('Ctrl Pts',(90.6986619011323,0.647482235274794,2.10674696036414));
#14093=CARTESIAN_POINT('Ctrl Pts',(90.69459339391,0.718843589872206,2.08481494372605));
#14094=CARTESIAN_POINT('Ctrl Pts',(90.6905248866878,0.789228822454979,2.05921012796652));
#14095=CARTESIAN_POINT('Ctrl Pts',(90.6864563794656,0.858232167974168,2.03003781882367));
#14096=CARTESIAN_POINT('Ctrl Pts',(90.6823938680067,0.927133823190694,2.0009085009434));
#14097=CARTESIAN_POINT('Ctrl Pts',(90.6783313565478,0.994657197189147,1.96822231187987));
#14098=CARTESIAN_POINT('Ctrl Pts',(90.6742688450889,1.06041176445151,1.93213428358715));
#14099=CARTESIAN_POINT('Ctrl Pts',(90.6702110880305,1.12608937844223,1.89608848949899));
#14100=CARTESIAN_POINT('Ctrl Pts',(90.6661533309721,1.19000188064749,1.85664899444771));
#14101=CARTESIAN_POINT('Ctrl Pts',(90.6620955739137,1.25178034377629,1.81401818373888));
#14102=CARTESIAN_POINT('Ctrl Pts',(90.6580403905352,1.31351962319224,1.77141441212039));
#14103=CARTESIAN_POINT('Ctrl Pts',(90.6539852071567,1.37312715631856,1.72562361233344));
#14104=CARTESIAN_POINT('Ctrl Pts',(90.6499300237782,1.43026135950486,1.67689249610919));
#14105=CARTESIAN_POINT('Ctrl Pts',(90.6458760942468,1.48737789701539,1.62817644735856));
#14106=CARTESIAN_POINT('Ctrl Pts',(90.6418221647154,1.54202225889323,1.5765221974819));
#14107=CARTESIAN_POINT('Ctrl Pts',(90.637768235184,1.59388573328848,1.52221689296218));
#14108=CARTESIAN_POINT('Ctrl Pts',(90.6337142413437,1.64575003041188,1.46791072697873));
#14109=CARTESIAN_POINT('Ctrl Pts',(90.6296602475034,1.69483302317828,1.41095377023961));
#14110=CARTESIAN_POINT('Ctrl Pts',(90.6256062536631,1.74086383325701,1.3516690105413));
#14111=CARTESIAN_POINT('Ctrl Pts',(90.6215480517177,1.78694242399259,1.2923227123918));
#14112=CARTESIAN_POINT('Ctrl Pts',(90.6174898497722,1.82996221123045,1.23064416509488));
#14113=CARTESIAN_POINT('Ctrl Pts',(90.6134316478268,1.86969399292404,1.1669877346501));
#14114=CARTESIAN_POINT('Ctrl Pts',(90.6093712990548,1.9094467931002,1.10329762936072));
#14115=CARTESIAN_POINT('Ctrl Pts',(90.6053109502827,1.94590789183945,1.03762797640211));
#14116=CARTESIAN_POINT('Ctrl Pts',(90.6012506015106,1.97889400045801,0.970357941664474));
#14117=CARTESIAN_POINT('Ctrl Pts',(90.5971829001436,2.01193984125961,0.902966092435923));
#14118=CARTESIAN_POINT('Ctrl Pts',(90.5931151987766,2.04149793453685,0.833968513628197));
#14119=CARTESIAN_POINT('Ctrl Pts',(90.5890474974096,2.06743327901196,0.763764123819556));
#14120=CARTESIAN_POINT('Ctrl Pts',(90.5858687266441,2.08770087178042,0.708901772383852));
#14121=CARTESIAN_POINT('Ctrl Pts',(90.5826899558786,2.10575706487792,0.65330285978906));
#14122=CARTESIAN_POINT('Ctrl Pts',(90.5795111851131,2.12155908224672,0.597162507644661));
#14123=CARTESIAN_POINT('Ctrl Pts',(90.5754307648268,2.14184329806247,0.525098100152149));
#14124=CARTESIAN_POINT('Ctrl Pts',(90.5713503445405,2.15849006587881,0.451862267806355));
#14125=CARTESIAN_POINT('Ctrl Pts',(90.5672699242542,2.17136853336895,0.377855385425647));
#14126=CARTESIAN_POINT('Ctrl Pts',(90.5631955068217,2.18422805488017,0.303957377244081));
#14127=CARTESIAN_POINT('Ctrl Pts',(90.5591210893891,2.1933302027879,0.229291036095995));
#14128=CARTESIAN_POINT('Ctrl Pts',(90.5550466719565,2.19859422016187,0.154270720069698));
#14129=CARTESIAN_POINT('Ctrl Pts',(90.5509770756259,2.203852008826,0.0793391727055896));
#14130=CARTESIAN_POINT('Ctrl Pts',(90.5469074792952,2.20528065798668,0.00405495480358915));
#14131=CARTESIAN_POINT('Ctrl Pts',(90.5428378829645,2.20285093137833,-0.0711602004328078));
#14132=CARTESIAN_POINT('Ctrl Pts',(90.5387709070012,2.20042276924367,-0.146326925474719));
#14133=CARTESIAN_POINT('Ctrl Pts',(90.5347039310379,2.19414117723868,-0.221424201966485));
#14134=CARTESIAN_POINT('Ctrl Pts',(90.5306369550746,2.18402899022925,-0.296029339488884));
#14135=CARTESIAN_POINT('Ctrl Pts',(90.5265712960636,2.17392007770856,-0.370610318668107));
#14136=CARTESIAN_POINT('Ctrl Pts',(90.5225056370525,2.1599830970921,-0.444699004357614));
#14137=CARTESIAN_POINT('Ctrl Pts',(90.5184399780414,2.14229267328171,-0.517878462579325));
#14138=CARTESIAN_POINT('Ctrl Pts',(90.5143743342984,2.12460231590537,-0.59105764598521));
#14139=CARTESIAN_POINT('Ctrl Pts',(90.5103086905554,2.10315865683447,-0.663327146850329));
#14140=CARTESIAN_POINT('Ctrl Pts',(90.5062430468124,2.07808694434501,-0.734282405987527));
#14141=CARTESIAN_POINT('Ctrl Pts',(90.502173398398,2.05299053614314,-0.805307556268941));
#14142=CARTESIAN_POINT('Ctrl Pts',(90.4981037499836,2.02425909656417,-0.87501543016943));
#14143=CARTESIAN_POINT('Ctrl Pts',(90.4940341015693,1.99206683038161,-0.943019481926743));
#14144=CARTESIAN_POINT('Ctrl Pts',(90.4899624013569,1.95985833379771,-1.01105781934278));
#14145=CARTESIAN_POINT('Ctrl Pts',(90.4858907011445,1.92418576047148,-1.07739020419027));
#14146=CARTESIAN_POINT('Ctrl Pts',(90.4818190009322,1.88526907726728,-1.14165516085189));
#14147=CARTESIAN_POINT('Ctrl Pts',(90.4777402319407,1.84628483176121,-1.20603168633299));
#14148=CARTESIAN_POINT('Ctrl Pts',(90.4736614629492,1.80404549352595,-1.26833321975903));
#14149=CARTESIAN_POINT('Ctrl Pts',(90.4695826939577,1.75881383871552,-1.3282280981604));
#14150=CARTESIAN_POINT('Ctrl Pts',(90.4665086190031,1.72472377441067,-1.37336949890708));
#14151=CARTESIAN_POINT('Ctrl Pts',(90.4634345440486,1.68893488061178,-1.41714447270139));
#14152=CARTESIAN_POINT('Ctrl Pts',(90.460360469094,1.65157360542284,-1.45942475855064));
#14153=CARTESIAN_POINT('Ctrl Pts',(90.4563285283101,1.60257075044973,-1.51487936242095));
#14154=CARTESIAN_POINT('Ctrl Pts',(90.4522965875262,1.55066908945272,-1.56797917703271));
#14155=CARTESIAN_POINT('Ctrl Pts',(90.4482646467423,1.49612610620718,-1.61840127110842));
#14156=CARTESIAN_POINT('Ctrl Pts',(90.4441648682423,1.44066543304279,-1.66967172082342));
#14157=CARTESIAN_POINT('Ctrl Pts',(90.4400650897423,1.38247400094061,-1.7181730728207));
#14158=CARTESIAN_POINT('Ctrl Pts',(90.4359653112423,1.32186546120693,-1.76360077751973));
#14159=CARTESIAN_POINT('Ctrl Pts',(90.4319438182175,1.26241424456713,-1.80816103792821));
#14160=CARTESIAN_POINT('Ctrl Pts',(90.4279223251928,1.20063782125386,-1.84976368663127));
#14161=CARTESIAN_POINT('Ctrl Pts',(90.4239008321681,1.13686783732387,-1.88815982386517));
#14162=CARTESIAN_POINT('Ctrl Pts',(90.4198816825718,1.07313501382011,-1.92653358667247));
#14163=CARTESIAN_POINT('Ctrl Pts',(90.4158625329755,1.00741135105409,-1.96170429303847));
#14164=CARTESIAN_POINT('Ctrl Pts',(90.4118433833792,0.940057517603746,-1.99346629356924));
#14165=CARTESIAN_POINT('Ctrl Pts',(90.4078252133142,0.872720099363314,-2.02522055319086));
#14166=CARTESIAN_POINT('Ctrl Pts',(90.4038070432492,0.803753740473402,-2.05356754842303));
#14167=CARTESIAN_POINT('Ctrl Pts',(90.3997888731841,0.73354218103753,-2.07834835112854));
#14168=CARTESIAN_POINT('Ctrl Pts',(90.3956289639807,0.660853940480139,-2.10400328548316));
#14169=CARTESIAN_POINT('Ctrl Pts',(90.3914690547772,0.586831519709844,-2.12583550938633));
#14170=CARTESIAN_POINT('Ctrl Pts',(90.3873091455737,0.511919365077974,-2.1437244607594));
#14171=CARTESIAN_POINT('Ctrl Pts',(90.3832864722748,0.439478571430073,-2.16102325347684));
#14172=CARTESIAN_POINT('Ctrl Pts',(90.3792637989758,0.366206342913574,-2.17463487349386));
#14173=CARTESIAN_POINT('Ctrl Pts',(90.3752411256769,0.292514097319783,-2.18450257561514));
#14174=CARTESIAN_POINT('Ctrl Pts',(90.3710125985211,0.21505076920307,-2.19487524157232));
#14175=CARTESIAN_POINT('Ctrl Pts',(90.3667840713654,0.137123900085511,-2.20111050061073));
#14176=CARTESIAN_POINT('Ctrl Pts',(90.3625555442096,0.0592135968959411,
-2.20320442763323));
#14177=CARTESIAN_POINT('Ctrl Pts',(90.3583270170539,-0.018696706293629,
-2.20529835465572));
#14178=CARTESIAN_POINT('Ctrl Pts',(90.3540984898981,-0.0965898279897558,
-2.20325104327665));
#14179=CARTESIAN_POINT('Ctrl Pts',(90.3498699627424,-0.173992556915814,
-2.19712143272462));
#14180=CARTESIAN_POINT('Ctrl Pts',(90.3498698986825,-0.173992556915814,
-2.19712143272462));
#14181=CARTESIAN_POINT('Ctrl Pts',(90.3498698986825,-0.18736228019796,-2.19593968129474));
#14182=CARTESIAN_POINT('Ctrl Pts',(90.3498698986825,-0.200732003480107,
-2.19475792986486));
#14183=CARTESIAN_POINT('Ctrl Pts',(90.3498698986825,-0.214101726762253,
-2.19357617843498));
#14184=CARTESIAN_POINT('Origin',(88.3562164250559,0.,0.));
#14185=CARTESIAN_POINT('',(99.9812164250558,-0.00144200395415034,1.77624941467256));
#14186=CARTESIAN_POINT('Ctrl Pts',(99.7906304259995,1.77562736014833,-0.0475451276259355));
#14187=CARTESIAN_POINT('Ctrl Pts',(99.8210626774041,1.7831651598518,0.405131671463454));
#14188=CARTESIAN_POINT('Ctrl Pts',(99.8845910813172,1.43986119934285,1.36540427831042));
#14189=CARTESIAN_POINT('Ctrl Pts',(99.9481194852301,0.490085748425745,1.77315870757737));
#14190=CARTESIAN_POINT('Ctrl Pts',(99.9812156377384,-0.00143133121117253,
1.77750555846212));
#14191=CARTESIAN_POINT('',(100.349866562796,-0.0937295438502085,-1.77377530569958));
#14192=CARTESIAN_POINT('Ctrl Pts',(99.9812164250558,-0.00144200395415034,
1.77624941467256));
#14193=CARTESIAN_POINT('Ctrl Pts',(99.9878369154481,-0.0996938618182821,
1.77616965134294));
#14194=CARTESIAN_POINT('Ctrl Pts',(99.9944574058404,-0.197622103560606,
1.7679352862269));
#14195=CARTESIAN_POINT('Ctrl Pts',(100.001077896233,-0.294176170481509,
1.75172042381792));
#14196=CARTESIAN_POINT('Ctrl Pts',(100.005371895501,-0.356800397409599,
1.74120358847903));
#14197=CARTESIAN_POINT('Ctrl Pts',(100.009665894769,-0.418989179132037,
1.72730256288422));
#14198=CARTESIAN_POINT('Ctrl Pts',(100.013959894037,-0.480348386519703,
1.71006710104251));
#14199=CARTESIAN_POINT('Ctrl Pts',(100.018387757296,-0.543620446671693,
1.69229432944351));
#14200=CARTESIAN_POINT('Ctrl Pts',(100.022815620555,-0.606009799062529,
1.67097574429));
#14201=CARTESIAN_POINT('Ctrl Pts',(100.027243483814,-0.667092358067373,
1.6462235110422));
#14202=CARTESIAN_POINT('Ctrl Pts',(100.031525654997,-0.726165088785864,
1.62228571221467));
#14203=CARTESIAN_POINT('Ctrl Pts',(100.03580782618,-0.784015179020576,1.59513692650705));
#14204=CARTESIAN_POINT('Ctrl Pts',(100.040089997363,-0.840273973818524,
1.5649292991772));
#14205=CARTESIAN_POINT('Ctrl Pts',(100.044369556558,-0.896498452547865,
1.53474009753555));
#14206=CARTESIAN_POINT('Ctrl Pts',(100.048649115754,-0.951133116423197,
1.50149599247278));
#14207=CARTESIAN_POINT('Ctrl Pts',(100.052928674949,-1.00383183752556,1.46539609132482));
#14208=CARTESIAN_POINT('Ctrl Pts',(100.057207173385,-1.05651749638528,1.42930513812965));
#14209=CARTESIAN_POINT('Ctrl Pts',(100.061485671822,-1.10726774841054,1.39036007930979));
#14210=CARTESIAN_POINT('Ctrl Pts',(100.065764170258,-1.1557652101126,1.34880348516504));
#14211=CARTESIAN_POINT('Ctrl Pts',(100.070043157405,-1.20426821143078,1.30724214422387));
#14212=CARTESIAN_POINT('Ctrl Pts',(100.074322144552,-1.25051753036019,1.26306900710094));
#14213=CARTESIAN_POINT('Ctrl Pts',(100.0786011317,-1.29423019245069,1.2165657694712));
#14214=CARTESIAN_POINT('Ctrl Pts',(100.082884940889,-1.3379921148689,1.17001012678042));
#14215=CARTESIAN_POINT('Ctrl Pts',(100.087168750079,-1.37921133261949,1.12111951512464));
#14216=CARTESIAN_POINT('Ctrl Pts',(100.091452559268,-1.41764381670143,1.07021029310514));
#14217=CARTESIAN_POINT('Ctrl Pts',(100.095739280734,-1.45610242845962,1.0192664613095));
#14218=CARTESIAN_POINT('Ctrl Pts',(100.100026002199,-1.49177025680286,0.966301708503973));
#14219=CARTESIAN_POINT('Ctrl Pts',(100.104312723664,-1.52444711914087,0.911660596627439));
#14220=CARTESIAN_POINT('Ctrl Pts',(100.108606769025,-1.55717981014966,0.856926129990768));
#14221=CARTESIAN_POINT('Ctrl Pts',(100.112900814387,-1.58691110996872,0.800510038579124));
#14222=CARTESIAN_POINT('Ctrl Pts',(100.117194859749,-1.61348773066646,0.74277951337445));
#14223=CARTESIAN_POINT('Ctrl Pts',(100.118206110583,-1.61974654434729,0.729183932316125));
#14224=CARTESIAN_POINT('Ctrl Pts',(100.119217361417,-1.62583061331469,0.715515525215639));
#14225=CARTESIAN_POINT('Ctrl Pts',(100.120228612252,-1.63173833712494,0.701779211473773));
#14226=CARTESIAN_POINT('Ctrl Pts',(100.124535184851,-1.65689731907099,0.643280933535056));
#14227=CARTESIAN_POINT('Ctrl Pts',(100.12884175745,-1.67895697168689,0.58331082626553));
#14228=CARTESIAN_POINT('Ctrl Pts',(100.13314833005,-1.69774574538958,0.522229304531615));
#14229=CARTESIAN_POINT('Ctrl Pts',(100.137574621642,-1.71705683074985,0.459449769325994));
#14230=CARTESIAN_POINT('Ctrl Pts',(100.142000913235,-1.73291216433171,0.395496553854958));
#14231=CARTESIAN_POINT('Ctrl Pts',(100.146427204827,-1.74517774248642,0.330784990031285));
#14232=CARTESIAN_POINT('Ctrl Pts',(100.150721876997,-1.75707859358033,0.267997677814478));
#14233=CARTESIAN_POINT('Ctrl Pts',(100.155016549166,-1.76560009894012,0.204497020559692));
#14234=CARTESIAN_POINT('Ctrl Pts',(100.159311221335,-1.7706704910092,0.140677200602032));
#14235=CARTESIAN_POINT('Ctrl Pts',(100.163603221152,-1.77573772803597,0.0768970924121892));
#14236=CARTESIAN_POINT('Ctrl Pts',(100.16789522097,-1.77735807128689,0.0127987147216979));
#14237=CARTESIAN_POINT('Ctrl Pts',(100.172187220787,-1.7755114340142,-0.0512172840440753));
#14238=CARTESIAN_POINT('Ctrl Pts',(100.176478080179,-1.77366528741048,-0.115216273153953));
#14239=CARTESIAN_POINT('Ctrl Pts',(100.180768939572,-1.7683540036489,-0.179132425294061));
#14240=CARTESIAN_POINT('Ctrl Pts',(100.185059798964,-1.75960959918077,-0.242565704440833));
#14241=CARTESIAN_POINT('Ctrl Pts',(100.189351048018,-1.75086440061465,-0.306004744098857));
#14242=CARTESIAN_POINT('Ctrl Pts',(100.193642297073,-1.73868553421696,-0.36896032699504));
#14243=CARTESIAN_POINT('Ctrl Pts',(100.197933546127,-1.72315655021774,-0.431040097835106));
#14244=CARTESIAN_POINT('Ctrl Pts',(100.202229394063,-1.7076109239893,-0.493186398834279));
#14245=CARTESIAN_POINT('Ctrl Pts',(100.206525241998,-1.68870814086263,-0.554454527962565));
#14246=CARTESIAN_POINT('Ctrl Pts',(100.210821089934,-1.66658200046735,-0.614466026903244));
#14247=CARTESIAN_POINT('Ctrl Pts',(100.215119733224,-1.6444414623536,-0.674516575974281));
#14248=CARTESIAN_POINT('Ctrl Pts',(100.219418376514,-1.61907359253653,-0.733308407332166));
#14249=CARTESIAN_POINT('Ctrl Pts',(100.223717019804,-1.5906597058994,-0.790484511251187));
#14250=CARTESIAN_POINT('Ctrl Pts',(100.228022711847,-1.56219922724194,-0.847754370390336));
#14251=CARTESIAN_POINT('Ctrl Pts',(100.232328403891,-1.5306830169525,-0.903402782285414));
#14252=CARTESIAN_POINT('Ctrl Pts',(100.236634095934,-1.49633689103465,-0.957099770676374));
#14253=CARTESIAN_POINT('Ctrl Pts',(100.23754917338,-1.48903739890877,-0.968511850888292));
#14254=CARTESIAN_POINT('Ctrl Pts',(100.238464250825,-1.48161023276245,-0.979835905416706));
#14255=CARTESIAN_POINT('Ctrl Pts',(100.239379328271,-1.47405779327266,-0.991068960563359));
#14256=CARTESIAN_POINT('Ctrl Pts',(100.243634734529,-1.43893650552586,-1.04330630223483));
#14257=CARTESIAN_POINT('Ctrl Pts',(100.247890140788,-1.400957248599,-1.09378977273184));
#14258=CARTESIAN_POINT('Ctrl Pts',(100.252145547047,-1.36032286525451,-1.14218464565313));
#14259=CARTESIAN_POINT('Ctrl Pts',(100.256393671885,-1.31975801135417,-1.19049671016595));
#14260=CARTESIAN_POINT('Ctrl Pts',(100.260641796723,-1.27654737586528,-1.23672687879013));
#14261=CARTESIAN_POINT('Ctrl Pts',(100.264889921561,-1.23093680649601,-1.28056965484639));
#14262=CARTESIAN_POINT('Ctrl Pts',(100.269134011856,-1.18536955455418,-1.32437079238998));
#14263=CARTESIAN_POINT('Ctrl Pts',(100.27337810215,-1.13740725348595,-1.36578867404023));
#14264=CARTESIAN_POINT('Ctrl Pts',(100.277622192445,-1.08733459704232,-1.40455243283219));
#14265=CARTESIAN_POINT('Ctrl Pts',(100.281863854929,-1.03729058441089,-1.44329401701018));
#14266=CARTESIAN_POINT('Ctrl Pts',(100.286105517412,-0.985139015793631,
-1.47938417314215));
#14267=CARTESIAN_POINT('Ctrl Pts',(100.290347179896,-0.931198259671605,
-1.5125917703348));
#14268=CARTESIAN_POINT('Ctrl Pts',(100.294588017752,-0.877267990261508,
-1.54579291158337));
#14269=CARTESIAN_POINT('Ctrl Pts',(100.298828855607,-0.82154966262879,-1.57611233701221));
#14270=CARTESIAN_POINT('Ctrl Pts',(100.303069693462,-0.764389468949105,
-1.60336296647381));
#14271=CARTESIAN_POINT('Ctrl Pts',(100.307314102526,-0.707181140686356,
-1.63063654368285));
#14272=CARTESIAN_POINT('Ctrl Pts',(100.311558511589,-0.648528986995092,
-1.65483594102652));
#14273=CARTESIAN_POINT('Ctrl Pts',(100.315802920653,-0.588801348259254,
-1.67582130156771));
#14274=CARTESIAN_POINT('Ctrl Pts',(100.320049173466,-0.529047764143368,
-1.69681577804193));
#14275=CARTESIAN_POINT('Ctrl Pts',(100.324295426279,-0.468218259647601,
-1.71459329296513));
#14276=CARTESIAN_POINT('Ctrl Pts',(100.328541679092,-0.406695647801983,
-1.72906411464669));
#14277=CARTESIAN_POINT('Ctrl Pts',(100.332795245003,-0.345067078799047,
-1.74355985866303));
#14278=CARTESIAN_POINT('Ctrl Pts',(100.337048810914,-0.282743526677385,
-1.75473744840853));
#14279=CARTESIAN_POINT('Ctrl Pts',(100.341302376825,-0.22011620541515,-1.76255862841882));
#14280=CARTESIAN_POINT('Ctrl Pts',(100.344157105482,-0.178084645905708,
-1.76780771757689));
#14281=CARTESIAN_POINT('Ctrl Pts',(100.347011834139,-0.135916384823446,
-1.77154607556643));
#14282=CARTESIAN_POINT('Ctrl Pts',(100.349866562796,-0.0937295438502085,
-1.77377530569958));
#14283=CARTESIAN_POINT('',(100.349869898682,-1.70764710160359,-0.4888818250711));
#14284=CARTESIAN_POINT('Origin',(100.349869898682,0.,0.));
#14285=CARTESIAN_POINT('',(100.129086863397,0.00137170632050479,1.77624947035088));
#14286=CARTESIAN_POINT('Ctrl Pts',(100.129086863397,0.0013717063205048,
1.77624947035088));
#14287=CARTESIAN_POINT('Ctrl Pts',(100.133321543366,-0.0614516234439551,
1.77629798558477));
#14288=CARTESIAN_POINT('Ctrl Pts',(100.137556223336,-0.124412816603254,
1.77300913712713));
#14289=CARTESIAN_POINT('Ctrl Pts',(100.141790903305,-0.187116606352544,
1.76636673375806));
#14290=CARTESIAN_POINT('Ctrl Pts',(100.145973038684,-0.249042357382847,
1.75980675039947));
#14291=CARTESIAN_POINT('Ctrl Pts',(100.150155174062,-0.310716513623133,
1.7499760021445));
#14292=CARTESIAN_POINT('Ctrl Pts',(100.154337309441,-0.371757544232495,
1.73691116376349));
#14293=CARTESIAN_POINT('Ctrl Pts',(100.15851669033,-0.432758371246943,1.72385493030713));
#14294=CARTESIAN_POINT('Ctrl Pts',(100.162696071219,-0.493126381012677,
1.70756893339161));
#14295=CARTESIAN_POINT('Ctrl Pts',(100.166875452108,-0.55248794642649,1.68814132452039));
#14296=CARTESIAN_POINT('Ctrl Pts',(100.171053739036,-0.611833973827677,
1.66871880086599));
#14297=CARTESIAN_POINT('Ctrl Pts',(100.175232025963,-0.670173575397997,
1.64615646001032));
#14298=CARTESIAN_POINT('Ctrl Pts',(100.179410312891,-0.727148330130597,
1.62059228940788));
#14299=CARTESIAN_POINT('Ctrl Pts',(100.183686052038,-0.78545193480656,1.59443187320832));
#14300=CARTESIAN_POINT('Ctrl Pts',(100.187961791186,-0.84232567474615,1.56512802426334));
#14301=CARTESIAN_POINT('Ctrl Pts',(100.192237530334,-0.897409713425917,
1.53287960021289));
#14302=CARTESIAN_POINT('Ctrl Pts',(100.196421458131,-0.951310953100947,
1.50132363453668));
#14303=CARTESIAN_POINT('Ctrl Pts',(100.200605385927,-1.00349818563022,1.4669486694603));
#14304=CARTESIAN_POINT('Ctrl Pts',(100.204789313724,-1.05366400520113,1.42998469454869));
#14305=CARTESIAN_POINT('Ctrl Pts',(100.209110958547,-1.10548106920959,1.39180402351839));
#14306=CARTESIAN_POINT('Ctrl Pts',(100.213432603371,-1.15514082602271,1.35086129312065));
#14307=CARTESIAN_POINT('Ctrl Pts',(100.217754248194,-1.20234438202791,1.3074525037285));
#14308=CARTESIAN_POINT('Ctrl Pts',(100.222075893017,-1.24954793803311,1.26404371433635));
#14309=CARTESIAN_POINT('Ctrl Pts',(100.22639753784,-1.29429493562015,1.21816937064235));
#14310=CARTESIAN_POINT('Ctrl Pts',(100.230719182663,-1.33633294203061,1.17016166855004));
#14311=CARTESIAN_POINT('Ctrl Pts',(100.235133769944,-1.37927502912348,1.12112149989295));
#14312=CARTESIAN_POINT('Ctrl Pts',(100.239548357224,-1.41958668769332,1.06963211146007));
#14313=CARTESIAN_POINT('Ctrl Pts',(100.243962944504,-1.45698615668822,1.01599970557028));
#14314=CARTESIAN_POINT('Ctrl Pts',(100.248375734261,-1.49437039744277,0.962389137615333));
#14315=CARTESIAN_POINT('Ctrl Pts',(100.252788524019,-1.52884448547413,0.906637633133585));
#14316=CARTESIAN_POINT('Ctrl Pts',(100.257201313776,-1.5601656568966,0.849086088415297));
#14317=CARTESIAN_POINT('Ctrl Pts',(100.2616010349,-1.59139406955399,0.791704984647155));
#14318=CARTESIAN_POINT('Ctrl Pts',(100.266000756023,-1.61948795076751,0.732534878825622));
#14319=CARTESIAN_POINT('Ctrl Pts',(100.270400477146,-1.64424956134948,0.671943035161504));
#14320=CARTESIAN_POINT('Ctrl Pts',(100.274795966228,-1.66898735401991,0.611409474102507));
#14321=CARTESIAN_POINT('Ctrl Pts',(100.27919145531,-1.69039906627075,0.549457326576857));
#14322=CARTESIAN_POINT('Ctrl Pts',(100.283586944391,-1.70833399824872,0.48647611753049));
#14323=CARTESIAN_POINT('Ctrl Pts',(100.287979471106,-1.72625684286847,0.423537355059128));
#14324=CARTESIAN_POINT('Ctrl Pts',(100.292371997821,-1.74070743551343,0.359571361705321));
#14325=CARTESIAN_POINT('Ctrl Pts',(100.296764524535,-1.75158461763224,0.294983711031818));
#14326=CARTESIAN_POINT('Ctrl Pts',(100.301189972381,-1.76254332210949,0.229911988514088));
#14327=CARTESIAN_POINT('Ctrl Pts',(100.305615420226,-1.76987468773199,0.164209716463454));
#14328=CARTESIAN_POINT('Ctrl Pts',(100.310040868072,-1.77352778075399,0.098301950101844));
#14329=CARTESIAN_POINT('Ctrl Pts',(100.314432487141,-1.77715294899391,0.0328979924311582));
#14330=CARTESIAN_POINT('Ctrl Pts',(100.31882410621,-1.77715590345277,-0.0327078499729776));
#14331=CARTESIAN_POINT('Ctrl Pts',(100.32321572528,-1.77353911854442,-0.098097183918244));
#14332=CARTESIAN_POINT('Ctrl Pts',(100.327658087513,-1.76988054332853,-0.164242061929393));
#14333=CARTESIAN_POINT('Ctrl Pts',(100.332100449747,-1.76251803703616,-0.230164902592036));
#14334=CARTESIAN_POINT('Ctrl Pts',(100.336542811981,-1.75150823419927,-0.295436910409244));
#14335=CARTESIAN_POINT('Ctrl Pts',(100.340985174215,-1.74049843136238,-0.360708918226453));
#14336=CARTESIAN_POINT('Ctrl Pts',(100.345427536448,-1.72584144827217,-0.42532960905316));
#14337=CARTESIAN_POINT('Ctrl Pts',(100.349869898682,-1.7076471016036,-0.488881825071076));
#14338=CARTESIAN_POINT('Ctrl Pts',(99.9383713772532,1.77277786422444,-0.0474589613121508));
#14339=CARTESIAN_POINT('Ctrl Pts',(99.9563868350438,1.78061088145064,0.221455662094678));
#14340=CARTESIAN_POINT('Ctrl Pts',(100.014119198174,1.61989353132562,1.08753612952137));
#14341=CARTESIAN_POINT('Ctrl Pts',(100.077691015475,0.763768868856085,1.73402760988346));
#14342=CARTESIAN_POINT('Ctrl Pts',(100.123247374986,0.0880846415247775,
1.77868931994825));
#14343=CARTESIAN_POINT('Ctrl Pts',(100.129086829157,0.00137347567789877,
1.77788227080619));
#14344=CARTESIAN_POINT('Origin',(25.4947388265965,0.,-6.40787078036307));
#14345=CARTESIAN_POINT('',(25.4947388265965,-7.48009298981943E-16,6.107959450045));
#14346=CARTESIAN_POINT('Origin',(25.4947388265965,0.,0.));
#14347=CARTESIAN_POINT('',(25.4947388265965,-7.47987577963046E-16,6.10778208446569));
#14348=CARTESIAN_POINT('Origin',(25.4947388265965,0.,0.));
#14349=CARTESIAN_POINT('Origin',(27.4542764744824,0.,0.));
#14350=CARTESIAN_POINT('',(27.7542764744824,-7.48069377062962E-16,6.10845002480549));
#14351=CARTESIAN_POINT('Origin',(27.7542764744824,0.,0.));
#14352=CARTESIAN_POINT('',(27.4541877916966,-7.84808779432149E-16,6.40845001169777));
#14353=CARTESIAN_POINT('Origin',(27.4542764744824,-7.48069377062961E-16,
6.10845002480549));
#14354=CARTESIAN_POINT('Origin',(27.4541877916966,-7.84808779432149E-16,
0.));
#14355=CARTESIAN_POINT('Origin',(26.6245076505395,0.,0.));
#14356=CARTESIAN_POINT('',(25.7946501438108,-7.8474870135113E-16,6.40795943693727));
#14357=CARTESIAN_POINT('',(26.6245076505395,-7.84778743602106E-16,6.40820475053297));
#14358=CARTESIAN_POINT('Origin',(25.7946501438108,-7.8474870135113E-16,
0.));
#14359=CARTESIAN_POINT('Origin',(25.7947388265966,0.,0.));
#14360=CARTESIAN_POINT('Origin',(25.7947388265966,-7.48009298981944E-16,
6.107959450045));
#14361=CARTESIAN_POINT('Origin',(27.7542764744824,0.,-6.40853872070288));
#14362=CARTESIAN_POINT('',(27.7542764744824,-7.4809109808186E-16,6.1086273903848));
#14363=CARTESIAN_POINT('Origin',(27.7542764744824,0.,0.));
#14364=CARTESIAN_POINT('Ctrl Pts',(90.1010424233136,1.30583205915545,-1.19933150781794));
#14365=CARTESIAN_POINT('Ctrl Pts',(90.1407593286533,1.70488751242686,-0.764839959096196));
#14366=CARTESIAN_POINT('Ctrl Pts',(90.2201931393327,2.02794301306985,0.526632618699088));
#14367=CARTESIAN_POINT('Ctrl Pts',(90.3393438553519,0.654151350163486,1.99272616320641));
#14368=CARTESIAN_POINT('Ctrl Pts',(90.4584945713711,-1.31950283566344,1.628071155055));
#14369=CARTESIAN_POINT('Ctrl Pts',(90.5776452873901,-2.08378435372669,-0.226191237424723));
#14370=CARTESIAN_POINT('Ctrl Pts',(90.6967960034093,-0.938691037125564,
-1.8743255371654));
#14371=CARTESIAN_POINT('Ctrl Pts',(90.8159467194284,1.06664039468703,-1.80433079412335));
#14372=CARTESIAN_POINT('Ctrl Pts',(90.9350974354475,2.09451613140419,-0.0812095856050628));
#14373=CARTESIAN_POINT('Ctrl Pts',(91.0542481514668,1.20307845886324,1.71647344469004));
#14374=CARTESIAN_POINT('Ctrl Pts',(91.1733988674858,-0.790818539461979,
1.94117803796467));
#14375=CARTESIAN_POINT('Ctrl Pts',(91.292549583505,-2.06003807063084,0.387103249808451));
#14376=CARTESIAN_POINT('Ctrl Pts',(91.4117002995241,-1.44152521409774,-1.52171537550226));
#14377=CARTESIAN_POINT('Ctrl Pts',(91.5308510155432,0.49794312834491,-2.03608731373934));
#14378=CARTESIAN_POINT('Ctrl Pts',(91.6500017315624,1.9811163478004,-0.68467704960091));
#14379=CARTESIAN_POINT('Ctrl Pts',(91.7691524475815,1.64887612811511,1.29414546959417));
#14380=CARTESIAN_POINT('Ctrl Pts',(91.8883031636006,-0.194326599410635,
2.08706505065828));
#14381=CARTESIAN_POINT('Ctrl Pts',(92.0074538796198,-1.8594563484299,0.967484492317832));
#14382=CARTESIAN_POINT('Ctrl Pts',(92.1266045956389,-1.82065667436397,-1.0386594260208));
#14383=CARTESIAN_POINT('Ctrl Pts',(92.2457553116581,-0.113481959304491,
-2.09301834340466));
#14384=CARTESIAN_POINT('Ctrl Pts',(92.3649060276773,1.69768295626714,-1.22942125805054));
#14385=CARTESIAN_POINT('Ctrl Pts',(92.4840567436963,1.95316091651168,0.760767028860157));
#14386=CARTESIAN_POINT('Ctrl Pts',(92.6032074597155,0.418842401989782,2.05381962675591));
#14387=CARTESIAN_POINT('Ctrl Pts',(92.7223581757346,-1.49928609228867,1.46483625188328));
#14388=CARTESIAN_POINT('Ctrl Pts',(92.8415088917537,-2.04353036839276,-0.466462927017294));
#14389=CARTESIAN_POINT('Ctrl Pts',(92.9606596077729,-0.715167316040089,
-1.97031462884506));
#14390=CARTESIAN_POINT('Ctrl Pts',(93.0798103237921,1.26854570192717,-1.66865090134507));
#14391=CARTESIAN_POINT('Ctrl Pts',(93.1989610398111,2.08981552149063,0.162096002811901));
#14392=CARTESIAN_POINT('Ctrl Pts',(93.3181117558304,0.99606419884773,1.84430478488173));
#14393=CARTESIAN_POINT('Ctrl Pts',(93.4372624718494,-1.01043946011796,1.83646838400132));
#14394=CARTESIAN_POINT('Ctrl Pts',(93.5564131878686,-2.09101788353122,0.145767755972613));
#14395=CARTESIAN_POINT('Ctrl Pts',(93.6755639038877,-1.25547336955694,-1.67850845879349));
#14396=CARTESIAN_POINT('Ctrl Pts',(93.7947146199069,0.730535394209225,-1.96466843659299));
#14397=CARTESIAN_POINT('Ctrl Pts',(93.9138653359261,2.04711151637174,-0.450486922634485));
#14398=CARTESIAN_POINT('Ctrl Pts',(94.033016051945,1.48779869334798,1.47650231154474));
#14399=CARTESIAN_POINT('Ctrl Pts',(94.1521667679643,-0.434871767592548,
2.0504854482974));
#14400=CARTESIAN_POINT('Ctrl Pts',(94.2713174839834,-1.95904359527549,0.745487907170205));
#14401=CARTESIAN_POINT('Ctrl Pts',(94.3904682000025,-1.6880283048537,-1.24264414453198));
#14402=CARTESIAN_POINT('Ctrl Pts',(94.5096189160217,0.129826818626143,-2.09206812152299));
#14403=CARTESIAN_POINT('Ctrl Pts',(94.6287696320409,1.82871397582683,-1.0244067661543));
#14404=CARTESIAN_POINT('Ctrl Pts',(94.74792034806,1.85184272723222,0.981978890569559));
#14405=CARTESIAN_POINT('Ctrl Pts',(94.8670710640791,0.178018834653386,2.08851940915947));
#14406=CARTESIAN_POINT('Ctrl Pts',(94.9862217800982,-1.65893420906864,1.28122648969999));
#14407=CARTESIAN_POINT('Ctrl Pts',(95.1053724961174,-1.97570805459144,-0.700129781504567));
#14408=CARTESIAN_POINT('Ctrl Pts',(95.2245232121365,-0.48202415568645,-2.03991586622143));
#14409=CARTESIAN_POINT('Ctrl Pts',(95.3436739281557,1.45336688898623,-1.51040680411788));
#14410=CARTESIAN_POINT('Ctrl Pts',(95.4628246441747,2.05695218758971,0.403177040389243));
#14411=CARTESIAN_POINT('Ctrl Pts',(95.5819753601939,0.775630953932477,1.94730599835489));
#14412=CARTESIAN_POINT('Ctrl Pts',(95.7011260762131,-1.21644664076787,1.70700369012245));
#14413=CARTESIAN_POINT('Ctrl Pts',(95.8202767922322,-2.0938224776132,-0.0975267151544407));
#14414=CARTESIAN_POINT('Ctrl Pts',(95.9394275082513,-1.05250536220669,-1.81268764282583));
#14415=CARTESIAN_POINT('Ctrl Pts',(96.0585782242705,0.953284454331289,-1.86677603826951));
#14416=CARTESIAN_POINT('Ctrl Pts',(96.1777289402896,2.08552353599421,-0.210227516612779));
#14417=CARTESIAN_POINT('Ctrl Pts',(96.2968796563088,1.30667447477482,1.63896486994091));
#14418=CARTESIAN_POINT('Ctrl Pts',(96.4160303723279,-0.669557426892749,
1.98627714078819));
#14419=CARTESIAN_POINT('Ctrl Pts',(96.5351810883469,-2.03223439262648,0.513446590555013));
#14420=CARTESIAN_POINT('Ctrl Pts',(96.6543318043663,-1.53265519856506,-1.42988533465054));
#14421=CARTESIAN_POINT('Ctrl Pts',(96.7734825203852,0.371386293120647,-2.06292904608715));
#14422=CARTESIAN_POINT('Ctrl Pts',(96.8926332364044,1.9351046338199,-0.805589277546201));
#14423=CARTESIAN_POINT('Ctrl Pts',(97.0117839524236,1.72557253784195,1.18995942983182));
#14424=CARTESIAN_POINT('Ctrl Pts',(97.1309346684427,-0.065203384874652,
2.09507817189829));
#14425=CARTESIAN_POINT('Ctrl Pts',(97.2500853844619,-1.79622960269954,1.08035329516627));
#14426=CARTESIAN_POINT('Ctrl Pts',(97.3692361004811,-1.88126476065518,-0.924362985387572));
#14427=CARTESIAN_POINT('Ctrl Pts',(97.4883868165,-0.242386130970125,-2.0820309772158));
#14428=CARTESIAN_POINT('Ctrl Pts',(97.6075375325194,1.61860519705063,-1.33181126474651));
#14429=CARTESIAN_POINT('Ctrl Pts',(97.7266882485383,1.99637317852867,0.638825612677669));
#14430=CARTESIAN_POINT('Ctrl Pts',(97.8458389645576,0.544746742790172,2.02406892253496));
#14431=CARTESIAN_POINT('Ctrl Pts',(97.9649896805767,-1.40606323902093,1.55453858294462));
#14432=CARTESIAN_POINT('Ctrl Pts',(98.0841403965958,-2.0684146040356,-0.339507106786872));
#14433=CARTESIAN_POINT('Ctrl Pts',(98.203291112615,-0.835355735837929,-1.9224423880883));
#14434=CARTESIAN_POINT('Ctrl Pts',(98.3224418286341,1.16318880525659,-1.74373046440489));
#14435=CARTESIAN_POINT('Ctrl Pts',(98.4415925446532,2.09583493445023,0.03286460299083));
#14436=CARTESIAN_POINT('Ctrl Pts',(98.5607432606724,1.10794387479709,1.77934362145635));
#14437=CARTESIAN_POINT('Ctrl Pts',(98.6798939766915,-0.895221256089004,
1.89530574973682));
#14438=CARTESIAN_POINT('Ctrl Pts',(98.7990446927107,-2.07804279474277,0.274486409481149));
#14439=CARTESIAN_POINT('Ctrl Pts',(98.9181954087297,-1.35663041470257,-1.59785882547245));
#14440=CARTESIAN_POINT('Ctrl Pts',(99.0373461247489,0.607940744949202,-2.00599618084136));
#14441=CARTESIAN_POINT('Ctrl Pts',(99.156496840768,2.01542321899274,-0.575912342987758));
#14442=CARTESIAN_POINT('Ctrl Pts',(99.2756475567872,1.57604812382197,1.38189668529539));
#14443=CARTESIAN_POINT('Ctrl Pts',(99.3947982728063,-0.307539860164324,
2.07342665626661));
#14444=CARTESIAN_POINT('Ctrl Pts',(99.5139489888255,-1.9093366442722,0.864885194893485));
#14445=CARTESIAN_POINT('Ctrl Pts',(99.6330997048446,-1.76144452875313,-1.13606536710066));
#14446=CARTESIAN_POINT('Ctrl Pts',(99.7522504208638,0.000461070801624738,
-2.09624351397064));
#14447=CARTESIAN_POINT('Ctrl Pts',(99.8714011368828,1.76214729717201,-1.13496987263683));
#14448=CARTESIAN_POINT('Ctrl Pts',(99.990551852902,1.90866885759355,0.865266786198645));
#14449=CARTESIAN_POINT('Ctrl Pts',(100.109702568921,0.306980077402089,2.07476137965942));
#14450=CARTESIAN_POINT('Ctrl Pts',(100.228868133282,-1.57796936803118,1.37855338932855));
#14451=CARTESIAN_POINT('Ctrl Pts',(100.308316792305,-1.86701861863313,0.0786761327033587));
#14452=CARTESIAN_POINT('Ctrl Pts',(100.348048545986,-1.70435785524601,-0.488628385190746));
#14453=CARTESIAN_POINT('Ctrl Pts',(90.1845168795555,1.41231704226503,-1.29713182942698));
#14454=CARTESIAN_POINT('Ctrl Pts',(90.2242337848953,1.84391374990636,-0.827209365295778));
#14455=CARTESIAN_POINT('Ctrl Pts',(90.3036675955747,2.19331303594521,0.569577241718508));
#14456=CARTESIAN_POINT('Ctrl Pts',(90.4228183115938,0.707494576794279,2.15522440357605));
#14457=CARTESIAN_POINT('Ctrl Pts',(90.541969027613,-1.4271026117476,1.76083334926806));
#14458=CARTESIAN_POINT('Ctrl Pts',(90.6611197436321,-2.25370799754816,-0.244636159134078));
#14459=CARTESIAN_POINT('Ctrl Pts',(90.7802704596512,-1.01523725034848,-2.02716871616958));
#14460=CARTESIAN_POINT('Ctrl Pts',(90.8994211756703,1.15362032722573,-1.95146620314416));
#14461=CARTESIAN_POINT('Ctrl Pts',(91.0185718916896,2.26531490549736,-0.0878318777220926));
#14462=CARTESIAN_POINT('Ctrl Pts',(91.1377226077086,1.30118432820023,1.85644446507076));
#14463=CARTESIAN_POINT('Ctrl Pts',(91.2568733237279,-0.855306387058394,
2.099472750624));
#14464=CARTESIAN_POINT('Ctrl Pts',(91.3760240397469,-2.22802530728827,0.418669853437552));
#14465=CARTESIAN_POINT('Ctrl Pts',(91.4951747557661,-1.55907538986423,-1.64580471373058));
#14466=CARTESIAN_POINT('Ctrl Pts',(91.6143254717852,0.538548246927779,-2.20212146927492));
#14467=CARTESIAN_POINT('Ctrl Pts',(91.7334761878043,2.14266785770134,-0.740509515614525));
#14468=CARTESIAN_POINT('Ctrl Pts',(91.8526269038236,1.78333487832047,1.39967746163317));
#14469=CARTESIAN_POINT('Ctrl Pts',(91.9717776198425,-0.210173097060069,
2.25725622119186));
#14470=CARTESIAN_POINT('Ctrl Pts',(92.0909283358618,-2.01108700910122,1.0463786878623));
#14471=CARTESIAN_POINT('Ctrl Pts',(92.2100790518808,-1.96912338863914,-1.12335763101657));
#14472=CARTESIAN_POINT('Ctrl Pts',(92.3292297679001,-0.12273592457137,-2.2636949793341));
#14473=CARTESIAN_POINT('Ctrl Pts',(92.4483804839192,1.83612169320582,-1.3296752692614));
#14474=CARTESIAN_POINT('Ctrl Pts',(92.5675311999383,2.11243278133292,0.822804305132014));
#14475=CARTESIAN_POINT('Ctrl Pts',(92.6866819159575,0.452997196849331,2.22129977608434));
#14476=CARTESIAN_POINT('Ctrl Pts',(92.8058326319765,-1.62154641902396,1.58428734243238));
#14477=CARTESIAN_POINT('Ctrl Pts',(92.9249833479958,-2.21017147299464,-0.504500970697111));
#14478=CARTESIAN_POINT('Ctrl Pts',(93.0441340640148,-0.773486132028051,
-2.13098530506418));
#14479=CARTESIAN_POINT('Ctrl Pts',(93.163284780034,1.37199014311418,-1.80472219918136));
#14480=CARTESIAN_POINT('Ctrl Pts',(93.2824354960531,2.26023098108043,0.175314234054207));
#14481=CARTESIAN_POINT('Ctrl Pts',(93.4015862120723,1.07728894643049,1.99469990076979));
#14482=CARTESIAN_POINT('Ctrl Pts',(93.5207369280913,-1.09283644837499,1.98622447513156));
#14483=CARTESIAN_POINT('Ctrl Pts',(93.6398876441106,-2.26153139056953,0.157654488974653));
#14484=CARTESIAN_POINT('Ctrl Pts',(93.7590383601297,-1.35785181831264,-1.8153835980051));
#14485=CARTESIAN_POINT('Ctrl Pts',(93.8781890761489,0.790107410815714,-2.12487869013955));
#14486=CARTESIAN_POINT('Ctrl Pts',(93.9973397921678,2.21404464817526,-0.487222191930033));
#14487=CARTESIAN_POINT('Ctrl Pts',(94.1164905081872,1.60912227215037,1.59690471903944));
#14488=CARTESIAN_POINT('Ctrl Pts',(94.2356412242062,-0.470333688214142,
2.21769370972545));
#14489=CARTESIAN_POINT('Ctrl Pts',(94.3547919402254,-2.11879516722628,0.80627923684147));
#14490=CARTESIAN_POINT('Ctrl Pts',(94.4739426562444,-1.82567974653074,-1.34397642521381));
#14491=CARTESIAN_POINT('Ctrl Pts',(94.5930933722636,0.140413636809712,-2.26266727094848));
#14492=CARTESIAN_POINT('Ctrl Pts',(94.7122440882828,1.9778377283514,-1.10794272809251));
#14493=CARTESIAN_POINT('Ctrl Pts',(94.8313948043019,2.00285252986982,1.0620550418963));
#14494=CARTESIAN_POINT('Ctrl Pts',(94.9505455203211,0.192535504288173,2.25882917636812));
#14495=CARTESIAN_POINT('Ctrl Pts',(95.0696962363401,-1.79421315247794,1.38570499454195));
#14496=CARTESIAN_POINT('Ctrl Pts',(95.1888469523594,-2.13681854146269,-0.757222351284346));
#14497=CARTESIAN_POINT('Ctrl Pts',(95.3079976683784,-0.521331150576662,
-2.20626222373084));
#14498=CARTESIAN_POINT('Ctrl Pts',(95.4271483843976,1.57188270236409,-1.6335739770307));
#14499=CARTESIAN_POINT('Ctrl Pts',(95.5462991004167,2.22468778376917,0.436054392446108));
#14500=CARTESIAN_POINT('Ctrl Pts',(95.6654498164359,0.838880319308144,2.10610041980454));
#14501=CARTESIAN_POINT('Ctrl Pts',(95.784600532455,-1.31564262779213,1.84620249278336));
#14502=CARTESIAN_POINT('Ctrl Pts',(95.9037512484742,-2.26456468722573,-0.105479598944601));
#14503=CARTESIAN_POINT('Ctrl Pts',(96.0229019644932,-1.1383326436948,-1.96050451688395));
#14504=CARTESIAN_POINT('Ctrl Pts',(96.1420526805125,1.03102069790592,-2.01900358813764));
#14505=CARTESIAN_POINT('Ctrl Pts',(96.2612033965315,2.25558900264279,-0.227370665610191));
#14506=CARTESIAN_POINT('Ctrl Pts',(96.3803541125507,1.41322815325176,1.77261539970789));
#14507=CARTESIAN_POINT('Ctrl Pts',(96.4995048285698,-0.724156952761073,
2.14824949114124));
#14508=CARTESIAN_POINT('Ctrl Pts',(96.618655544589,-2.19795435903126,0.555315949742211));
#14509=CARTESIAN_POINT('Ctrl Pts',(96.737806260608,-1.65763663227069,-1.54648632835516));
#14510=CARTESIAN_POINT('Ctrl Pts',(96.8569569766272,0.401671246589807,-2.23115202934803));
#14511=CARTESIAN_POINT('Ctrl Pts',(96.9761076926464,2.09290408651586,-0.871281615248694));
#14512=CARTESIAN_POINT('Ctrl Pts',(97.0952584086655,1.86628555009966,1.28699549882576));
#14513=CARTESIAN_POINT('Ctrl Pts',(97.2144091246847,-0.0705204402251945,
2.2659227779743));
#14514=CARTESIAN_POINT('Ctrl Pts',(97.3335598407038,-1.94270439443354,1.16845145570812));
#14515=CARTESIAN_POINT('Ctrl Pts',(97.452710556723,-2.03467380346316,-0.99974080767029));
#14516=CARTESIAN_POINT('Ctrl Pts',(97.571861272742,-0.262151676532748,-2.25181164073069));
#14517=CARTESIAN_POINT('Ctrl Pts',(97.6910119887613,1.75059548313724,-1.44041474023738));
#14518=CARTESIAN_POINT('Ctrl Pts',(97.8101627047803,2.15916881729827,0.690919091390331));
#14519=CARTESIAN_POINT('Ctrl Pts',(97.9293134207995,0.589168494652002,2.18912303000429));
#14520=CARTESIAN_POINT('Ctrl Pts',(98.0484641368186,-1.52072164337573,1.68130451244333));
#14521=CARTESIAN_POINT('Ctrl Pts',(98.1676148528378,-2.23708491093308,-0.36719244984327));
#14522=CARTESIAN_POINT('Ctrl Pts',(98.2867655688569,-0.903475400076174,
-2.07920928915298));
#14523=CARTESIAN_POINT('Ctrl Pts',(98.405916284876,1.25804184505795,-1.885924177408));
#14524=CARTESIAN_POINT('Ctrl Pts',(98.5250670008952,2.26674125125465,0.0355445698899612));
#14525=CARTESIAN_POINT('Ctrl Pts',(98.6442177169143,1.19829192833657,1.92444143411032));
#14526=CARTESIAN_POINT('Ctrl Pts',(98.7633684329336,-0.968222695796038,
2.0498597747611));
#14527=CARTESIAN_POINT('Ctrl Pts',(98.8825191489526,-2.24749823914522,0.296869594571833));
#14528=CARTESIAN_POINT('Ctrl Pts',(99.0016698649718,-1.46725778503147,-1.72815733426533));
#14529=CARTESIAN_POINT('Ctrl Pts',(99.1208205809907,0.657515695651045,-2.16957653402469));
#14530=CARTESIAN_POINT('Ctrl Pts',(99.2399712970101,2.17977230655602,-0.622875515384769));
#14531=CARTESIAN_POINT('Ctrl Pts',(99.359122013029,1.70456806378548,1.49458441122548));
#14532=CARTESIAN_POINT('Ctrl Pts',(99.4782727290483,-0.332618411870491,
2.24250567444778));
#14533=CARTESIAN_POINT('Ctrl Pts',(99.5974234450674,-2.06503482834595,0.935412859400004));
#14534=CARTESIAN_POINT('Ctrl Pts',(99.7165741610866,-1.90508274744876,-1.22870660728074));
#14535=CARTESIAN_POINT('Ctrl Pts',(99.8357248771057,0.000498669140674738,
-2.2671831486761));
#14536=CARTESIAN_POINT('Ctrl Pts',(99.9548755931249,1.90584282360693,-1.22752177995927));
#14537=CARTESIAN_POINT('Ctrl Pts',(100.074026309144,2.06431258653835,0.935825567833403));
#14538=CARTESIAN_POINT('Ctrl Pts',(100.193177025163,0.332012981233764,2.24394923878758));
#14539=CARTESIAN_POINT('Ctrl Pts',(100.312342589524,-1.70664597718939,1.49096848386471));
#14540=CARTESIAN_POINT('Ctrl Pts',(100.391791248547,-2.01926594988565,0.0850918326422001));
#14541=CARTESIAN_POINT('Ctrl Pts',(100.431523002228,-1.84334090146247,-0.528473926567276));
#14542=CARTESIAN_POINT('Ctrl Pts',(90.2679913357975,1.51880202537459,-1.394932151036));
#14543=CARTESIAN_POINT('Ctrl Pts',(90.3077082411372,1.98293998738585,-0.889578771495359));
#14544=CARTESIAN_POINT('Ctrl Pts',(90.3871420518166,2.35868305882058,0.612521864737925));
#14545=CARTESIAN_POINT('Ctrl Pts',(90.5062927678359,0.76083780342507,2.3177226439457));
#14546=CARTESIAN_POINT('Ctrl Pts',(90.6254434838548,-1.53470238783176,1.89359554348111));
#14547=CARTESIAN_POINT('Ctrl Pts',(90.7445941998742,-2.42363164136963,-0.263081080843427));
#14548=CARTESIAN_POINT('Ctrl Pts',(90.8637449158931,-1.09178346357141,-2.18001189517376));
#14549=CARTESIAN_POINT('Ctrl Pts',(90.9828956319124,1.24060025976444,-2.09860161216497));
#14550=CARTESIAN_POINT('Ctrl Pts',(91.1020463479315,2.43611367959052,-0.0944541698391232));
#14551=CARTESIAN_POINT('Ctrl Pts',(91.2211970639506,1.39929019753722,1.99641548545147));
#14552=CARTESIAN_POINT('Ctrl Pts',(91.3403477799699,-0.919794234654806,
2.25776746328333));
#14553=CARTESIAN_POINT('Ctrl Pts',(91.4594984959889,-2.39601254394569,0.450236457066652));
#14554=CARTESIAN_POINT('Ctrl Pts',(91.578649212008,-1.67662556563072,-1.7698940519589));
#14555=CARTESIAN_POINT('Ctrl Pts',(91.6977999280273,0.579153365510643,-2.3681556248105));
#14556=CARTESIAN_POINT('Ctrl Pts',(91.8169506440462,2.30421936760228,-0.796341981628139));
#14557=CARTESIAN_POINT('Ctrl Pts',(91.9361013600655,1.91779362852583,1.50520945367216));
#14558=CARTESIAN_POINT('Ctrl Pts',(92.0552520760845,-0.226019594709503,
2.42744739172543));
#14559=CARTESIAN_POINT('Ctrl Pts',(92.1744027921037,-2.16271766977255,1.12527288340679));
#14560=CARTESIAN_POINT('Ctrl Pts',(92.293553508123,-2.11759010291431,-1.20805583601235));
#14561=CARTESIAN_POINT('Ctrl Pts',(92.412704224142,-0.131989889838248,-2.43437161526355));
#14562=CARTESIAN_POINT('Ctrl Pts',(92.5318549401611,1.97456043014449,-1.42992928047227));
#14563=CARTESIAN_POINT('Ctrl Pts',(92.6510056561803,2.27170464615415,0.884841581403872));
#14564=CARTESIAN_POINT('Ctrl Pts',(92.7701563721993,0.487151991708878,2.38877992541277));
#14565=CARTESIAN_POINT('Ctrl Pts',(92.8893070882187,-1.74380674575924,1.70373843298149));
#14566=CARTESIAN_POINT('Ctrl Pts',(93.0084578042377,-2.37681257759652,-0.542539014376926));
#14567=CARTESIAN_POINT('Ctrl Pts',(93.1276085202568,-0.831804948016011,
-2.29165598128329));
#14568=CARTESIAN_POINT('Ctrl Pts',(93.2467592362759,1.47543458430119,-1.94079349701765));
#14569=CARTESIAN_POINT('Ctrl Pts',(93.3659099522951,2.43064644067022,0.188532465296514));
#14570=CARTESIAN_POINT('Ctrl Pts',(93.4850606683143,1.15851369401324,2.14509501665785));
#14571=CARTESIAN_POINT('Ctrl Pts',(93.6042113843334,-1.17523343663204,2.13598056626179));
#14572=CARTESIAN_POINT('Ctrl Pts',(93.7233621003525,-2.43204489760782,0.169541221976694));
#14573=CARTESIAN_POINT('Ctrl Pts',(93.8425128163716,-1.46023026706835,-1.95225873721671));
#14574=CARTESIAN_POINT('Ctrl Pts',(93.9616635323908,0.849679427422205,-2.28508894368612));
#14575=CARTESIAN_POINT('Ctrl Pts',(94.0808142484098,2.38097777997878,-0.523957461225582));
#14576=CARTESIAN_POINT('Ctrl Pts',(94.1999649644292,1.73044585095274,1.71730712653414));
#14577=CARTESIAN_POINT('Ctrl Pts',(94.3191156804481,-0.505795608835735,
2.38490197115348));
#14578=CARTESIAN_POINT('Ctrl Pts',(94.4382663964674,-2.27854673917708,0.867070566512739));
#14579=CARTESIAN_POINT('Ctrl Pts',(94.5574171124865,-1.96333118820778,-1.44530870589565));
#14580=CARTESIAN_POINT('Ctrl Pts',(94.6765678285056,0.151000454993279,-2.43326642037397));
#14581=CARTESIAN_POINT('Ctrl Pts',(94.7957185445247,2.12696148087597,-1.19147869003071));
#14582=CARTESIAN_POINT('Ctrl Pts',(94.9148692605438,2.15386233250742,1.14213119322304));
#14583=CARTESIAN_POINT('Ctrl Pts',(95.034019976563,0.207052173922958,2.42913894357677));
#14584=CARTESIAN_POINT('Ctrl Pts',(95.1531706925822,-1.92949209588725,1.49018349938391));
#14585=CARTESIAN_POINT('Ctrl Pts',(95.2723214086013,-2.29792902833395,-0.814314921064122));
#14586=CARTESIAN_POINT('Ctrl Pts',(95.3914721246205,-0.560638145466874,
-2.37260858124027));
#14587=CARTESIAN_POINT('Ctrl Pts',(95.5106228406395,1.69039851574195,-1.75674114994351));
#14588=CARTESIAN_POINT('Ctrl Pts',(95.6297735566587,2.39242337994864,0.468931744502973));
#14589=CARTESIAN_POINT('Ctrl Pts',(95.7489242726778,0.90212968468381,2.26489484125418));
#14590=CARTESIAN_POINT('Ctrl Pts',(95.868074988697,-1.4148386148164,1.98540129544429));
#14591=CARTESIAN_POINT('Ctrl Pts',(95.9872257047161,-2.43530689683827,-0.113432482734765));
#14592=CARTESIAN_POINT('Ctrl Pts',(96.1063764207353,-1.22415992518291,-2.10832139094206));
#14593=CARTESIAN_POINT('Ctrl Pts',(96.2255271367545,1.10875694148055,-2.17123113800578));
#14594=CARTESIAN_POINT('Ctrl Pts',(96.3446778527735,2.42565446929138,-0.244513814607605));
#14595=CARTESIAN_POINT('Ctrl Pts',(96.4638285687928,1.51978183172869,1.90626592947487));
#14596=CARTESIAN_POINT('Ctrl Pts',(96.5829792848118,-0.778756478629395,
2.31022184149429));
#14597=CARTESIAN_POINT('Ctrl Pts',(96.7021300008311,-2.36367432543604,0.597185308929409));
#14598=CARTESIAN_POINT('Ctrl Pts',(96.8212807168501,-1.7826180659763,-1.66308732205977));
#14599=CARTESIAN_POINT('Ctrl Pts',(96.9404314328693,0.431956200058963,-2.39937501260893));
#14600=CARTESIAN_POINT('Ctrl Pts',(97.0595821488882,2.25070353921181,-0.936973952951183));
#14601=CARTESIAN_POINT('Ctrl Pts',(97.1787328649075,2.00699856235737,1.38403156781969));
#14602=CARTESIAN_POINT('Ctrl Pts',(97.2978835809267,-0.0758374955757388,
2.4367673840503));
#14603=CARTESIAN_POINT('Ctrl Pts',(97.4170342969457,-2.08917918616753,1.25654961624997));
#14604=CARTESIAN_POINT('Ctrl Pts',(97.536185012965,-2.18808284627115,-1.075118629953));
#14605=CARTESIAN_POINT('Ctrl Pts',(97.6553357289841,-0.281917222095369,
-2.42159230424558));
#14606=CARTESIAN_POINT('Ctrl Pts',(97.7744864450031,1.88258576922385,-1.54901821572826));
#14607=CARTESIAN_POINT('Ctrl Pts',(97.8936371610223,2.32196445606787,0.743012570102993));
#14608=CARTESIAN_POINT('Ctrl Pts',(98.0127878770415,0.633590246513833,2.35417713747362));
#14609=CARTESIAN_POINT('Ctrl Pts',(98.1319385930606,-1.63538004773054,1.80807044194204));
#14610=CARTESIAN_POINT('Ctrl Pts',(98.2510893090799,-2.40575521783057,-0.394877792899667));
#14611=CARTESIAN_POINT('Ctrl Pts',(98.370240025099,-0.971595064314421,-2.23597619021765));
#14612=CARTESIAN_POINT('Ctrl Pts',(98.489390741118,1.35289488485932,-2.02811789041112));
#14613=CARTESIAN_POINT('Ctrl Pts',(98.6085414571373,2.43764756805906,0.0382245367890935));
#14614=CARTESIAN_POINT('Ctrl Pts',(98.7276921731562,1.28863998187605,2.06953924676429));
#14615=CARTESIAN_POINT('Ctrl Pts',(98.8468428891755,-1.04122413550308,2.20441379978537));
#14616=CARTESIAN_POINT('Ctrl Pts',(98.9659936051947,-2.41695368354768,0.319252779662519));
#14617=CARTESIAN_POINT('Ctrl Pts',(99.0851443212136,-1.57788515536039,-1.85845584305822));
#14618=CARTESIAN_POINT('Ctrl Pts',(99.204295037233,0.70709064635289,-2.33315688720802));
#14619=CARTESIAN_POINT('Ctrl Pts',(99.323445753252,2.3441213941193,-0.669838687781786));
#14620=CARTESIAN_POINT('Ctrl Pts',(99.4425964692711,1.83308800374897,1.60727213715557));
#14621=CARTESIAN_POINT('Ctrl Pts',(99.5617471852904,-0.357696963576656,
2.41158469262895));
#14622=CARTESIAN_POINT('Ctrl Pts',(99.6808979013095,-2.22073301241972,1.00594052390652));
#14623=CARTESIAN_POINT('Ctrl Pts',(99.8000486173285,-2.0487209661444,-1.32134784746082));
#14624=CARTESIAN_POINT('Ctrl Pts',(99.9191993333478,0.00053626747972391,
-2.43812278338156));
#14625=CARTESIAN_POINT('Ctrl Pts',(100.038350049367,2.04953835004185,-1.32007368728171));
#14626=CARTESIAN_POINT('Ctrl Pts',(100.157500765386,2.21995631548315,1.00638434946817));
#14627=CARTESIAN_POINT('Ctrl Pts',(100.276651481405,0.357045885065439,2.41313709791574));
#14628=CARTESIAN_POINT('Ctrl Pts',(100.395817045766,-1.8353225863476,1.60338357840087));
#14629=CARTESIAN_POINT('Ctrl Pts',(100.475265704789,-2.17151328113818,0.0915075325810447));
#14630=CARTESIAN_POINT('Ctrl Pts',(100.51499745847,-1.98232394767894,-0.568319467943805));
#14631=CARTESIAN_POINT('Ctrl Pts',(90.3514657920395,1.62528700848416,-1.49273247264503));
#14632=CARTESIAN_POINT('Ctrl Pts',(90.3911826973793,2.12196622486536,-0.951948177694941));
#14633=CARTESIAN_POINT('Ctrl Pts',(90.4706165080587,2.52405308169595,0.655466487757345));
#14634=CARTESIAN_POINT('Ctrl Pts',(90.5897672240778,0.814181030055862,2.48022088431535));
#14635=CARTESIAN_POINT('Ctrl Pts',(90.708917940097,-1.64230216391592,2.02635773769416));
#14636=CARTESIAN_POINT('Ctrl Pts',(90.828068656116,-2.5935552851911,-0.281526002552781));
#14637=CARTESIAN_POINT('Ctrl Pts',(90.9472193721352,-1.16832967679433,-2.33285507417793));
#14638=CARTESIAN_POINT('Ctrl Pts',(91.0663700881543,1.32758019230315,-2.24573702118577));
#14639=CARTESIAN_POINT('Ctrl Pts',(91.1855208041735,2.60691245368369,-0.101076461956154));
#14640=CARTESIAN_POINT('Ctrl Pts',(91.3046715201927,1.49739606687422,2.13638650583218));
#14641=CARTESIAN_POINT('Ctrl Pts',(91.4238222362116,-0.98428208225122,2.41606217594266));
#14642=CARTESIAN_POINT('Ctrl Pts',(91.5429729522309,-2.56399978060312,0.481803060695756));
#14643=CARTESIAN_POINT('Ctrl Pts',(91.6621236682501,-1.79417574139721,-1.89398339018722));
#14644=CARTESIAN_POINT('Ctrl Pts',(91.7812743842692,0.61975848409351,-2.53418978034607));
#14645=CARTESIAN_POINT('Ctrl Pts',(91.9004251002883,2.46577087750323,-0.852174447641754));
#14646=CARTESIAN_POINT('Ctrl Pts',(92.0195758163074,2.05225237873119,1.61074144571115));
#14647=CARTESIAN_POINT('Ctrl Pts',(92.1387265323266,-0.241866092358935,
2.597638562259));
#14648=CARTESIAN_POINT('Ctrl Pts',(92.2578772483458,-2.31434833044387,1.20416707895126));
#14649=CARTESIAN_POINT('Ctrl Pts',(92.3770279643649,-2.26605681718948,-1.29275404100813));
#14650=CARTESIAN_POINT('Ctrl Pts',(92.4961786803841,-0.141243855105126,
-2.605048251193));
#14651=CARTESIAN_POINT('Ctrl Pts',(92.6153293964031,2.11299916708316,-1.53018329168314));
#14652=CARTESIAN_POINT('Ctrl Pts',(92.7344801124224,2.43097651097537,0.946878857675728));
#14653=CARTESIAN_POINT('Ctrl Pts',(92.8536308284414,0.521306786568425,2.55626007474121));
#14654=CARTESIAN_POINT('Ctrl Pts',(92.9727815444605,-1.86606707249453,1.82318952353058));
#14655=CARTESIAN_POINT('Ctrl Pts',(93.0919322604797,-2.5434536821984,-0.580577058056743));
#14656=CARTESIAN_POINT('Ctrl Pts',(93.2110829764989,-0.890123764003973,
-2.45232665750241));
#14657=CARTESIAN_POINT('Ctrl Pts',(93.3302336925179,1.5788790254882,-2.07686479485395));
#14658=CARTESIAN_POINT('Ctrl Pts',(93.4493844085372,2.60106190026,0.201750696538821));
#14659=CARTESIAN_POINT('Ctrl Pts',(93.5685351245561,1.23973844159599,2.29549013254591));
#14660=CARTESIAN_POINT('Ctrl Pts',(93.6876858405755,-1.25763042488907,2.28573665739201));
#14661=CARTESIAN_POINT('Ctrl Pts',(93.8068365565945,-2.60255840464611,0.181427954978733));
#14662=CARTESIAN_POINT('Ctrl Pts',(93.9259872726136,-1.56260871582405,-2.08913387642833));
#14663=CARTESIAN_POINT('Ctrl Pts',(94.0451379886329,0.909251444028696,-2.44529919723268));
#14664=CARTESIAN_POINT('Ctrl Pts',(94.1642887046518,2.54791091178229,-0.560692730521131));
#14665=CARTESIAN_POINT('Ctrl Pts',(94.2834394206712,1.85176942975512,1.83770953402883));
#14666=CARTESIAN_POINT('Ctrl Pts',(94.4025901366902,-0.541257529457329,
2.55211023258152));
#14667=CARTESIAN_POINT('Ctrl Pts',(94.5217408527093,-2.43829831112787,0.927861896184007));
#14668=CARTESIAN_POINT('Ctrl Pts',(94.6408915687285,-2.10098262988481,-1.54664098657749));
#14669=CARTESIAN_POINT('Ctrl Pts',(94.7600422847476,0.161587273176848,-2.60386556979946));
#14670=CARTESIAN_POINT('Ctrl Pts',(94.8791930007667,2.27608523340055,-1.27501465196891));
#14671=CARTESIAN_POINT('Ctrl Pts',(94.9983437167859,2.30487213514503,1.22220734454978));
#14672=CARTESIAN_POINT('Ctrl Pts',(95.1174944328051,0.221568843557745,2.59944871078543));
#14673=CARTESIAN_POINT('Ctrl Pts',(95.2366451488242,-2.06477103929656,1.59466200422586));
#14674=CARTESIAN_POINT('Ctrl Pts',(95.3557958648434,-2.45903951520519,-0.871407490843901));
#14675=CARTESIAN_POINT('Ctrl Pts',(95.4749465808624,-0.599945140357085,
-2.53895493874968));
#14676=CARTESIAN_POINT('Ctrl Pts',(95.5940972968817,1.80891432911982,-1.87990832285632));
#14677=CARTESIAN_POINT('Ctrl Pts',(95.7132480129007,2.5601589761281,0.501809096559839));
#14678=CARTESIAN_POINT('Ctrl Pts',(95.8323987289199,0.965379050059475,2.42368926270382));
#14679=CARTESIAN_POINT('Ctrl Pts',(95.951549444939,-1.51403460184066,2.1246000981052));
#14680=CARTESIAN_POINT('Ctrl Pts',(96.0707001609581,-2.60604910645081,-0.121385366524927));
#14681=CARTESIAN_POINT('Ctrl Pts',(96.1898508769773,-1.30998720667102,-2.25613826500018));
#14682=CARTESIAN_POINT('Ctrl Pts',(96.3090015929964,1.18649318505518,-2.32345868787391));
#14683=CARTESIAN_POINT('Ctrl Pts',(96.4281523090155,2.59571993593996,-0.261656963605017));
#14684=CARTESIAN_POINT('Ctrl Pts',(96.5473030250347,1.62633551020562,2.03991645924184));
#14685=CARTESIAN_POINT('Ctrl Pts',(96.6664537410539,-0.833356004497719,
2.47219419184734));
#14686=CARTESIAN_POINT('Ctrl Pts',(96.7856044570729,-2.52939429184081,0.639054668116608));
#14687=CARTESIAN_POINT('Ctrl Pts',(96.9047551730922,-1.90759949968193,-1.77968831576439));
#14688=CARTESIAN_POINT('Ctrl Pts',(97.0239058891112,0.462241153528123,-2.56759799586982));
#14689=CARTESIAN_POINT('Ctrl Pts',(97.1430566051304,2.40850299190777,-1.00266629065368));
#14690=CARTESIAN_POINT('Ctrl Pts',(97.2622073211496,2.14771157461508,1.48106763681363));
#14691=CARTESIAN_POINT('Ctrl Pts',(97.3813580371687,-0.0811545509262814,
2.60761199012629));
#14692=CARTESIAN_POINT('Ctrl Pts',(97.5005087531878,-2.23565397790152,1.34464777679182));
#14693=CARTESIAN_POINT('Ctrl Pts',(97.6196594692069,-2.34149188907913,-1.15049645223572));
#14694=CARTESIAN_POINT('Ctrl Pts',(97.738810185226,-0.301682767657992,-2.59137296776048));
#14695=CARTESIAN_POINT('Ctrl Pts',(97.8579609012452,2.01457605531046,-1.65762169121913));
#14696=CARTESIAN_POINT('Ctrl Pts',(97.9771116172644,2.48476009483747,0.795106048815653));
#14697=CARTESIAN_POINT('Ctrl Pts',(98.0962623332834,0.678011998375664,2.51923124494296));
#14698=CARTESIAN_POINT('Ctrl Pts',(98.2154130493027,-1.75003845208536,1.93483637144075));
#14699=CARTESIAN_POINT('Ctrl Pts',(98.3345637653216,-2.57442552472806,-0.422563135956064));
#14700=CARTESIAN_POINT('Ctrl Pts',(98.453714481341,-1.03971472855267,-2.39274309128233));
#14701=CARTESIAN_POINT('Ctrl Pts',(98.57286519736,1.44774792466069,-2.17031160341423));
#14702=CARTESIAN_POINT('Ctrl Pts',(98.6920159133792,2.60855388486348,0.0409045036882235));
#14703=CARTESIAN_POINT('Ctrl Pts',(98.8111666293983,1.37898803541552,2.21463705941828));
#14704=CARTESIAN_POINT('Ctrl Pts',(98.9303173454174,-1.11422557521011,2.35896782480965));
#14705=CARTESIAN_POINT('Ctrl Pts',(99.0494680614366,-2.58640912795013,0.341635964753205));
#14706=CARTESIAN_POINT('Ctrl Pts',(99.1686187774558,-1.68851252568929,-1.98875435185111));
#14707=CARTESIAN_POINT('Ctrl Pts',(99.2877694934747,0.756665597054732,-2.49673724039136));
#14708=CARTESIAN_POINT('Ctrl Pts',(99.4069202094941,2.50847048168259,-0.7168018601788));
#14709=CARTESIAN_POINT('Ctrl Pts',(99.5260709255131,1.96160794371247,1.71995986308567));
#14710=CARTESIAN_POINT('Ctrl Pts',(99.6452216415324,-0.382775515282821,
2.58066371081011));
#14711=CARTESIAN_POINT('Ctrl Pts',(99.7643723575514,-2.37643119649348,1.07646818841304));
#14712=CARTESIAN_POINT('Ctrl Pts',(99.8835230735704,-2.19235918484003,-1.4139890876409));
#14713=CARTESIAN_POINT('Ctrl Pts',(100.00267378959,0.000573865818775353,
-2.60906241808703));
#14714=CARTESIAN_POINT('Ctrl Pts',(100.121824505609,2.19323387647676,-1.41262559460416));
#14715=CARTESIAN_POINT('Ctrl Pts',(100.240975221628,2.37560004442796,1.07694313110293));
#14716=CARTESIAN_POINT('Ctrl Pts',(100.360125937647,0.382078788897115,2.58232495704388));
#14717=CARTESIAN_POINT('Ctrl Pts',(100.479291502008,-1.96399919550581,1.71579867293704));
#14718=CARTESIAN_POINT('Ctrl Pts',(100.558740161031,-2.3237606123907,0.0979232325198861));
#14719=CARTESIAN_POINT('Ctrl Pts',(100.598471914712,-2.12130699389541,-0.608165009320335));
#14720=CARTESIAN_POINT('Ctrl Pts',(100.349869898682,0.479414994925344,2.1549256777475));
#14721=CARTESIAN_POINT('Ctrl Pts',(100.349869898682,0.426652918711055,2.16183856744942));
#14722=CARTESIAN_POINT('Ctrl Pts',(100.349869898682,0.373742092670611,2.16669187525483));
#14723=CARTESIAN_POINT('Ctrl Pts',(100.349869898682,0.320765011501748,2.16941984999741));
#14724=CARTESIAN_POINT('Ctrl Pts',(100.349869898682,0.243016014531923,2.173423417112));
#14725=CARTESIAN_POINT('Ctrl Pts',(100.349869898682,0.165123647545959,2.17285169457002));
#14726=CARTESIAN_POINT('Ctrl Pts',(100.349869898682,0.0874187568974411,
2.16789484102177));
#14727=CARTESIAN_POINT('Ctrl Pts',(100.349869898682,0.00882392244760108,
2.1628812172876));
#14728=CARTESIAN_POINT('Ctrl Pts',(100.349869898682,-0.0695801138469986,
2.1533809621849));
#14729=CARTESIAN_POINT('Ctrl Pts',(100.349869898682,-0.147434733752325,
2.13954043578746));
#14730=CARTESIAN_POINT('Ctrl Pts',(100.349869898682,-0.214042289520903,
2.12769934485407));
#14731=CARTESIAN_POINT('Ctrl Pts',(100.349869898682,-0.280247772593053,
2.11268039049434));
#14732=CARTESIAN_POINT('Ctrl Pts',(100.349869898682,-0.345809014350891,
2.09455055013339));
#14733=CARTESIAN_POINT('Ctrl Pts',(100.349869898682,-0.357788807056832,
2.09123774330587));
#14734=CARTESIAN_POINT('Ctrl Pts',(100.349869898682,-0.369741677068317,
2.08782245032933));
#14735=CARTESIAN_POINT('Ctrl Pts',(100.349869898682,-0.381659087973615,
2.08430749424005));
#14736=CARTESIAN_POINT('Ctrl Pts',(100.349869898682,-0.455832595007861,
2.06243054275413));
#14737=CARTESIAN_POINT('Ctrl Pts',(100.349869898682,-0.528720372107131,
2.03667310777151));
#14738=CARTESIAN_POINT('Ctrl Pts',(100.349869898682,-0.599998286878196,
2.00720683894348));
#14739=CARTESIAN_POINT('Ctrl Pts',(100.349869898682,-0.67107164032602,1.97782513570582));
#14740=CARTESIAN_POINT('Ctrl Pts',(100.349869898682,-0.74054525402381,1.94475525164764));
#14741=CARTESIAN_POINT('Ctrl Pts',(100.349869898682,-0.808069062026671,
1.90812458172216));
#14742=CARTESIAN_POINT('Ctrl Pts',(100.349869898682,-0.875592870029532,
1.87149391179667));
#14743=CARTESIAN_POINT('Ctrl Pts',(100.349869898682,-0.941167756187684,
1.83130189691578));
#14744=CARTESIAN_POINT('Ctrl Pts',(100.349869898682,-1.00440156213994,1.78764176103566));
#14745=CARTESIAN_POINT('Ctrl Pts',(100.349869898682,-1.02779687561394,1.77148833566689));
#14746=CARTESIAN_POINT('Ctrl Pts',(100.349869898682,-1.05087124668119,1.75485987879237));
#14747=CARTESIAN_POINT('Ctrl Pts',(100.349869898682,-1.07360298298094,1.73776016033235));
#14748=CARTESIAN_POINT('Ctrl Pts',(100.349869898682,-1.08344175669883,1.73035904242613));
#14749=CARTESIAN_POINT('Ctrl Pts',(100.349869898682,-1.09320813055687,1.72287579541148));
#14750=CARTESIAN_POINT('Ctrl Pts',(100.349869898682,-1.10289990339264,1.71531171169833));
#14751=CARTESIAN_POINT('Ctrl Pts',(100.349869898682,-1.16103677699879,1.6699379512698));
#14752=CARTESIAN_POINT('Ctrl Pts',(100.349869898682,-1.2165025157906,1.62165059609133));
#14753=CARTESIAN_POINT('Ctrl Pts',(100.349869898682,-1.26898476684194,1.57056955349251));
#14754=CARTESIAN_POINT('Ctrl Pts',(100.349869898682,-1.31991541638646,1.52099868664032));
#14755=CARTESIAN_POINT('Ctrl Pts',(100.349869898682,-1.36803686611545,1.46879626038254));
#14756=CARTESIAN_POINT('Ctrl Pts',(100.349869898682,-1.41302321703878,1.41404528435321));
#14757=CARTESIAN_POINT('Ctrl Pts',(100.349869898682,-1.44122551224844,1.37972146930035));
#14758=CARTESIAN_POINT('Ctrl Pts',(100.349869898682,-1.46819484161769,1.34439554642142));
#14759=CARTESIAN_POINT('Ctrl Pts',(100.349869898682,-1.4938411634309,1.30808394627534));
#14760=CARTESIAN_POINT('Ctrl Pts',(100.349869898682,-1.51638234254341,1.27616879334555));
#14761=CARTESIAN_POINT('Ctrl Pts',(100.349869898682,-1.53790129532058,1.24349204802205));
#14762=CARTESIAN_POINT('Ctrl Pts',(100.349869898682,-1.55838417110218,1.21010641100884));
#14763=CARTESIAN_POINT('Ctrl Pts',(100.349869898682,-1.56666347577931,1.19661173069051));
#14764=CARTESIAN_POINT('Ctrl Pts',(100.349869898682,-1.57477345721915,1.18300122799903));
#14765=CARTESIAN_POINT('Ctrl Pts',(100.349869898682,-1.58271301197484,1.16927838686893));
#14766=CARTESIAN_POINT('Ctrl Pts',(100.349869898682,-1.58818639734872,1.15981810852325));
#14767=CARTESIAN_POINT('Ctrl Pts',(100.349869898682,-1.59357707452811,1.15030730513012));
#14768=CARTESIAN_POINT('Ctrl Pts',(100.349869898682,-1.59888102457648,1.14075431016918));
#14769=CARTESIAN_POINT('Ctrl Pts',(100.349869898682,-1.63352381179489,1.07835885608061));
#14770=CARTESIAN_POINT('Ctrl Pts',(100.349869898682,-1.66452248560101,1.01407626559023));
#14771=CARTESIAN_POINT('Ctrl Pts',(100.349869898682,-1.69186815495165,0.948254794836713));
#14772=CARTESIAN_POINT('Ctrl Pts',(100.349869898682,-1.71949907166491,0.881746729043388));
#14773=CARTESIAN_POINT('Ctrl Pts',(100.349869898682,-1.74340046295035,0.813666407902212));
#14774=CARTESIAN_POINT('Ctrl Pts',(100.349869898682,-1.76351145670095,0.744362695384729));
#14775=CARTESIAN_POINT('Ctrl Pts',(100.349869898682,-1.7781837869541,0.693800949384702));
#14776=CARTESIAN_POINT('Ctrl Pts',(100.349869898682,-1.79083752896901,0.642587752416721));
#14777=CARTESIAN_POINT('Ctrl Pts',(100.349869898682,-1.8014315909638,0.59086023556729));
#14778=CARTESIAN_POINT('Ctrl Pts',(100.349869898682,-1.80788893402677,0.559331033429673));
#14779=CARTESIAN_POINT('Ctrl Pts',(100.349869898682,-1.81358077732546,0.527610800354083));
#14780=CARTESIAN_POINT('Ctrl Pts',(100.349869898682,-1.81849513035574,0.495731460558739));
#14781=CARTESIAN_POINT('Ctrl Pts',(100.349869898682,-1.8204466171093,0.483072193115112));
#14782=CARTESIAN_POINT('Ctrl Pts',(100.349869898682,-1.82227577945555,0.470385589327682));
#14783=CARTESIAN_POINT('Ctrl Pts',(100.349869898682,-1.82398080210467,0.457681045001224));
#14784=CARTESIAN_POINT('Ctrl Pts',(100.349869898682,-1.83331587287951,0.388123130031295));
#14785=CARTESIAN_POINT('Ctrl Pts',(100.349869898682,-1.83891415245773,0.31818414364734));
#14786=CARTESIAN_POINT('Ctrl Pts',(100.349869898682,-1.84071131029323,0.248192856383627));
#14787=CARTESIAN_POINT('Ctrl Pts',(100.349869898682,-1.84233496365157,0.184958795148171));
#14788=CARTESIAN_POINT('Ctrl Pts',(100.349869898682,-1.84085536620268,0.121681523415235));
#14789=CARTESIAN_POINT('Ctrl Pts',(100.349869898682,-1.83619001506039,0.0586141186189351));
#14790=CARTESIAN_POINT('Ctrl Pts',(100.349869898682,-1.83446389372289,0.0352799708131937));
#14791=CARTESIAN_POINT('Ctrl Pts',(100.349869898682,-1.83230134629332,0.0119746999217489));
#14792=CARTESIAN_POINT('Ctrl Pts',(100.349869898682,-1.82969704876561,-0.0112882622057297));
#14793=CARTESIAN_POINT('Ctrl Pts',(100.349869898682,-1.82803245302949,-0.0261573112120898));
#14794=CARTESIAN_POINT('Ctrl Pts',(100.349869898682,-1.82618711014688,-0.0410101441524755));
#14795=CARTESIAN_POINT('Ctrl Pts',(100.349869898682,-1.8241621629289,-0.0558261756737762));
#14796=CARTESIAN_POINT('Ctrl Pts',(100.349869898682,-1.81512268037633,-0.121965805016011));
#14797=CARTESIAN_POINT('Ctrl Pts',(100.349869898682,-1.80249961741287,-0.187453075266988));
#14798=CARTESIAN_POINT('Ctrl Pts',(100.349869898682,-1.78620616216217,-0.251987814719906));
#14799=CARTESIAN_POINT('Ctrl Pts',(100.349869898682,-1.77003269803824,-0.316047296102442));
#14800=CARTESIAN_POINT('Ctrl Pts',(100.349869898682,-1.75024259013915,-0.379169001454444));
#14801=CARTESIAN_POINT('Ctrl Pts',(100.349869898682,-1.72670765863932,-0.441032704914043));
#14802=CARTESIAN_POINT('Ctrl Pts',(100.349869898682,-1.72060689789584,-0.457069108228638));
#14803=CARTESIAN_POINT('Ctrl Pts',(100.349869898682,-1.71425427817139,-0.473020805173385));
#14804=CARTESIAN_POINT('Ctrl Pts',(100.349869898682,-1.7076471016036,-0.488881825071076));
#14805=CARTESIAN_POINT('Ctrl Pts',(90.3498698986825,0.431841315399936,1.72595542684201));
#14806=CARTESIAN_POINT('Ctrl Pts',(90.3498698986825,0.474841144465498,1.72062771663674));
#14807=CARTESIAN_POINT('Ctrl Pts',(90.3498698986825,0.517549233669023,1.71363307981672));
#14808=CARTESIAN_POINT('Ctrl Pts',(90.3498698986825,0.559872741940156,1.70495472032253));
#14809=CARTESIAN_POINT('Ctrl Pts',(90.3498698986825,0.624504400694465,1.69170211456541));
#14810=CARTESIAN_POINT('Ctrl Pts',(90.3498698986825,0.688239505726174,1.67452610531829));
#14811=CARTESIAN_POINT('Ctrl Pts',(90.3498698986825,0.750879107325786,1.65371126257901));
#14812=CARTESIAN_POINT('Ctrl Pts',(90.3498698986825,0.785762674423698,1.64211961855852));
#14813=CARTESIAN_POINT('Ctrl Pts',(90.3498698986825,0.820306563194663,1.62939848267447));
#14814=CARTESIAN_POINT('Ctrl Pts',(90.3498698986825,0.85447616357889,1.61559006912156));
#14815=CARTESIAN_POINT('Ctrl Pts',(90.3498698986825,0.867794193387564,1.61020806695471));
#14816=CARTESIAN_POINT('Ctrl Pts',(90.3498698986825,0.881057426269837,1.60465994112489));
#14817=CARTESIAN_POINT('Ctrl Pts',(90.3498698986825,0.894257109673279,1.59895090028477));
#14818=CARTESIAN_POINT('Ctrl Pts',(90.3498698986825,0.956519137646987,1.5720217346657));
#14819=CARTESIAN_POINT('Ctrl Pts',(90.3498698986825,1.0172384297205,1.54157364190433));
#14820=CARTESIAN_POINT('Ctrl Pts',(90.3498698986825,1.076208979192,1.50790448231969));
#14821=CARTESIAN_POINT('Ctrl Pts',(90.3498698986825,1.13685273154978,1.47328000969319));
#14822=CARTESIAN_POINT('Ctrl Pts',(90.3498698986825,1.19564793846948,1.43524882235765));
#14823=CARTESIAN_POINT('Ctrl Pts',(90.3498698986825,1.25236316356456,1.39408084780544));
#14824=CARTESIAN_POINT('Ctrl Pts',(90.3498698986825,1.26444032963692,1.38531437522781));
#14825=CARTESIAN_POINT('Ctrl Pts',(90.3498698986825,1.27642312556602,1.37640548370778));
#14826=CARTESIAN_POINT('Ctrl Pts',(90.3498698986825,1.2883092163036,1.36735649508758));
#14827=CARTESIAN_POINT('Ctrl Pts',(90.3498698986825,1.30329584009537,1.3559470425484));
#14828=CARTESIAN_POINT('Ctrl Pts',(90.3498698986825,1.31813332928754,1.34431096898487));
#14829=CARTESIAN_POINT('Ctrl Pts',(90.3498698986825,1.3327907185954,1.33247444330209));
#14830=CARTESIAN_POINT('Ctrl Pts',(90.3498698986825,1.38844900248271,1.28752778241633));
#14831=CARTESIAN_POINT('Ctrl Pts',(90.3498698986825,1.44157223405924,1.23965136935539));
#14832=CARTESIAN_POINT('Ctrl Pts',(90.3498698986825,1.49193815705566,1.18915424604306));
#14833=CARTESIAN_POINT('Ctrl Pts',(90.3498698986825,1.54319438475154,1.13776449883903));
#14834=CARTESIAN_POINT('Ctrl Pts',(90.3498698986825,1.59159590601355,1.08366009580108));
#14835=CARTESIAN_POINT('Ctrl Pts',(90.3498698986825,1.63689108900039,1.0271159092752));
#14836=CARTESIAN_POINT('Ctrl Pts',(90.3498698986825,1.66837534617324,0.987812575171713));
#14837=CARTESIAN_POINT('Ctrl Pts',(90.3498698986825,1.69835842343872,0.947329379839982));
#14838=CARTESIAN_POINT('Ctrl Pts',(90.3498698986825,1.72674724367579,0.905746523557564));
#14839=CARTESIAN_POINT('Ctrl Pts',(90.3498698986825,1.74998131073704,0.871714152243922));
#14840=CARTESIAN_POINT('Ctrl Pts',(90.3498698986825,1.77214742214936,0.836945004136101));
#14841=CARTESIAN_POINT('Ctrl Pts',(90.3498698986825,1.79318980004415,0.801478956440622));
#14842=CARTESIAN_POINT('Ctrl Pts',(90.3498698986825,1.79955534257003,0.790750100797062));
#14843=CARTESIAN_POINT('Ctrl Pts',(90.3498698986825,1.80581833349576,0.779956701588121));
#14844=CARTESIAN_POINT('Ctrl Pts',(90.3498698986825,1.81196923948669,0.76911428545529));
#14845=CARTESIAN_POINT('Ctrl Pts',(90.3498698986825,1.84875184073078,0.704276313663116));
#14846=CARTESIAN_POINT('Ctrl Pts',(90.3498698986825,1.88159981518027,0.637570922779393));
#14847=CARTESIAN_POINT('Ctrl Pts',(90.3498698986825,1.91026209575641,0.569292558053354));
#14848=CARTESIAN_POINT('Ctrl Pts',(90.3498698986825,1.91921179749468,0.547972865858888));
#14849=CARTESIAN_POINT('Ctrl Pts',(90.3498698986825,1.92775318680489,0.526499495860395));
#14850=CARTESIAN_POINT('Ctrl Pts',(90.3498698986825,1.93587796203386,0.504880604295509));
#14851=CARTESIAN_POINT('Ctrl Pts',(90.3498698986825,1.96125429222846,0.437357735621538));
#14852=CARTESIAN_POINT('Ctrl Pts',(90.3498698986825,1.98257013429095,0.368417422671431));
#14853=CARTESIAN_POINT('Ctrl Pts',(90.3498698986825,1.99995022625151,0.298378990239349));
#14854=CARTESIAN_POINT('Ctrl Pts',(90.3498698986825,2.01733031821208,0.228340557807268));
#14855=CARTESIAN_POINT('Ctrl Pts',(90.3498698986825,2.03077467779787,0.157203167161219));
#14856=CARTESIAN_POINT('Ctrl Pts',(90.3498698986825,2.04036047300214,0.0852645536046794));
#14857=CARTESIAN_POINT('Ctrl Pts',(90.3498698986825,2.04251882481325,0.0690667490876812));
#14858=CARTESIAN_POINT('Ctrl Pts',(90.3498698986825,2.04448173438142,0.0528237008312664));
#14859=CARTESIAN_POINT('Ctrl Pts',(90.3498698986825,2.04624695875265,0.0365679053387175));
#14860=CARTESIAN_POINT('Ctrl Pts',(90.3498698986825,2.05428355565145,-0.0374404064496148));
#14861=CARTESIAN_POINT('Ctrl Pts',(90.3498698986825,2.05824267691487,-0.111815486997948));
#14862=CARTESIAN_POINT('Ctrl Pts',(90.3498698986825,2.05827617422769,-0.186215580692539));
#14863=CARTESIAN_POINT('Ctrl Pts',(90.3498698986825,2.05831029294706,-0.261995865846831));
#14864=CARTESIAN_POINT('Ctrl Pts',(90.3498698986825,2.05427191440473,-0.337802955333537));
#14865=CARTESIAN_POINT('Ctrl Pts',(90.3498698986825,2.04627147701347,-0.413297832907415));
#14866=CARTESIAN_POINT('Ctrl Pts',(90.3498698986825,2.03818548362252,-0.489600046306389));
#14867=CARTESIAN_POINT('Ctrl Pts',(90.3498698986825,2.02605230738084,-0.565584325900605));
#14868=CARTESIAN_POINT('Ctrl Pts',(90.3498698986825,2.00993395345466,-0.640908956253526));
#14869=CARTESIAN_POINT('Ctrl Pts',(90.3498698986825,2.00386961328568,-0.669248958195093));
#14870=CARTESIAN_POINT('Ctrl Pts',(90.3498698986825,1.9972406228178,-0.697495589008317));
#14871=CARTESIAN_POINT('Ctrl Pts',(90.3498698986825,1.99004837701446,-0.725630494083073));
#14872=CARTESIAN_POINT('Ctrl Pts',(90.3498698986825,1.98683004789391,-0.738220078307771));
#14873=CARTESIAN_POINT('Ctrl Pts',(90.3498698986825,1.98349864718324,-0.750787978975287));
#14874=CARTESIAN_POINT('Ctrl Pts',(90.3498698986825,1.98005882552643,-0.763316755998211));
#14875=CARTESIAN_POINT('Ctrl Pts',(90.3498698986825,1.95909233732488,-0.839682475456528));
#14876=CARTESIAN_POINT('Ctrl Pts',(90.3498698986825,1.93406748684242,-0.914733173091299));
#14877=CARTESIAN_POINT('Ctrl Pts',(90.3498698986825,1.90511090692207,-0.988108398984206));
#14878=CARTESIAN_POINT('Ctrl Pts',(90.3498698986825,1.87610067909659,-1.06161956728362));
#14879=CARTESIAN_POINT('Ctrl Pts',(90.3498698986825,1.84314408917545,-1.13345011151776));
#14880=CARTESIAN_POINT('Ctrl Pts',(90.3498698986825,1.80631634283528,-1.20323986437882));
#14881=CARTESIAN_POINT('Ctrl Pts',(90.3498698986825,1.77027623606683,-1.27153701515267));
#14882=CARTESIAN_POINT('Ctrl Pts',(90.3498698986825,1.73052856007642,-1.33788070102088));
#14883=CARTESIAN_POINT('Ctrl Pts',(90.3498698986825,1.68709628885172,-1.40192061396105));
#14884=CARTESIAN_POINT('Ctrl Pts',(90.3498698986825,1.66663353523406,-1.43209248670082));
#14885=CARTESIAN_POINT('Ctrl Pts',(90.3498698986825,1.6453522241745,-1.46175270636413));
#14886=CARTESIAN_POINT('Ctrl Pts',(90.3498698986825,1.62325119196239,-1.49086269246791));
#14887=CARTESIAN_POINT('Origin',(90.3498698986825,-2.40291074888303E-16,
0.));
#14888=CARTESIAN_POINT('Ctrl Pts',(90.3498698986825,-0.214101726762246,
-2.19357617843498));
#14889=CARTESIAN_POINT('Ctrl Pts',(90.3498698986825,-0.253065554508825,
-2.18618780244257));
#14890=CARTESIAN_POINT('Ctrl Pts',(90.3498698986825,-0.291777125231032,
-2.17767057969178));
#14891=CARTESIAN_POINT('Ctrl Pts',(90.3498698986825,-0.330194078040925,
-2.16800471972977));
#14892=CARTESIAN_POINT('Ctrl Pts',(90.3498698986825,-0.406738639552015,
-2.14874579994817));
#14893=CARTESIAN_POINT('Ctrl Pts',(90.3498698986825,-0.482115441140247,
-2.12492954084353));
#14894=CARTESIAN_POINT('Ctrl Pts',(90.3498698986825,-0.556039436073237,
-2.09682490939037));
#14895=CARTESIAN_POINT('Ctrl Pts',(90.3498698986825,-0.591892015170574,
-2.08319437544683));
#14896=CARTESIAN_POINT('Ctrl Pts',(90.3498698986825,-0.627402453816474,
-2.06855445598174));
#14897=CARTESIAN_POINT('Ctrl Pts',(90.3498698986825,-0.662535477352669,
-2.05293241695311));
#14898=CARTESIAN_POINT('Ctrl Pts',(90.3498698986825,-0.679780447079454,
-2.0452643723898));
#14899=CARTESIAN_POINT('Ctrl Pts',(90.3498698986825,-0.696934454724005,
-2.03735967383535));
#14900=CARTESIAN_POINT('Ctrl Pts',(90.3498698986825,-0.713993138554701,
-2.02922138301724));
#14901=CARTESIAN_POINT('Ctrl Pts',(90.3498698986825,-0.726153529799593,
-2.02341995065616));
#14902=CARTESIAN_POINT('Ctrl Pts',(90.3498698986825,-0.738263467090767,
-2.01750071137784));
#14903=CARTESIAN_POINT('Ctrl Pts',(90.3498698986825,-0.750313634121258,
-2.01146892060574));
#14904=CARTESIAN_POINT('Ctrl Pts',(90.3498698986825,-0.82032062923626,-1.9764264563769));
#14905=CARTESIAN_POINT('Ctrl Pts',(90.3498698986825,-0.888389925919542,
-1.93755209171669));
#14906=CARTESIAN_POINT('Ctrl Pts',(90.3498698986825,-0.954242008533983,
-1.89510921263127));
#14907=CARTESIAN_POINT('Ctrl Pts',(90.3498698986825,-1.00375379709209,-1.86319795376679));
#14908=CARTESIAN_POINT('Ctrl Pts',(90.3498698986825,-1.05201168240331,-1.82926838600246));
#14909=CARTESIAN_POINT('Ctrl Pts',(90.3498698986825,-1.09888241457234,-1.79341950884159));
#14910=CARTESIAN_POINT('Ctrl Pts',(90.3498698986825,-1.12145931356828,-1.7761516651079));
#14911=CARTESIAN_POINT('Ctrl Pts',(90.3498698986825,-1.14371416086655,-1.75843836186296));
#14912=CARTESIAN_POINT('Ctrl Pts',(90.3498698986825,-1.16563083104683,-1.7402899773242));
#14913=CARTESIAN_POINT('Ctrl Pts',(90.3498698986825,-1.17633935367306,-1.73142264552315));
#14914=CARTESIAN_POINT('Ctrl Pts',(90.3498698986825,-1.18696862372855,-1.72245015180797));
#14915=CARTESIAN_POINT('Ctrl Pts',(90.3498698986825,-1.19751194217376,-1.7133777644169));
#14916=CARTESIAN_POINT('Ctrl Pts',(90.3498698986825,-1.25555020267444,-1.66343660163185));
#14917=CARTESIAN_POINT('Ctrl Pts',(90.3498698986825,-1.31081695979071,-1.61061924093467));
#14918=CARTESIAN_POINT('Ctrl Pts',(90.3498698986825,-1.36305428432945,-1.55517048740135));
#14919=CARTESIAN_POINT('Ctrl Pts',(90.3498698986825,-1.41423592356646,-1.50084232024226));
#14920=CARTESIAN_POINT('Ctrl Pts',(90.3498698986825,-1.46250982432993,-1.44398719082985));
#14921=CARTESIAN_POINT('Ctrl Pts',(90.3498698986825,-1.50759196670537,-1.38480940415008));
#14922=CARTESIAN_POINT('Ctrl Pts',(90.3498698986825,-1.55169882705472,-1.32691183683546));
#14923=CARTESIAN_POINT('Ctrl Pts',(90.3498698986825,-1.5927509135165,-1.26679030648339));
#14924=CARTESIAN_POINT('Ctrl Pts',(90.3498698986825,-1.63043591394233,-1.20462243846731));
#14925=CARTESIAN_POINT('Ctrl Pts',(90.3498698986825,-1.64313694391478,-1.18366991236745));
#14926=CARTESIAN_POINT('Ctrl Pts',(90.3498698986825,-1.6554550854017,-1.16248487188985));
#14927=CARTESIAN_POINT('Ctrl Pts',(90.3498698986825,-1.66737704460729,-1.14107396752518));
#14928=CARTESIAN_POINT('Ctrl Pts',(90.3498698986825,-1.6741165542006,-1.12897033649619));
#14929=CARTESIAN_POINT('Ctrl Pts',(90.3498698986825,-1.6807294444079,-1.11679452622328));
#14930=CARTESIAN_POINT('Ctrl Pts',(90.3498698986825,-1.68721321125448,-1.10454773595022));
#14931=CARTESIAN_POINT('Ctrl Pts',(90.3498698986825,-1.69280679091001,-1.09398236576683));
#14932=CARTESIAN_POINT('Ctrl Pts',(90.3498698986825,-1.69830255810943,-1.08336726810866));
#14933=CARTESIAN_POINT('Ctrl Pts',(90.3498698986825,-1.7036947776161,-1.07271211575908));
#14934=CARTESIAN_POINT('Ctrl Pts',(90.3498698986825,-1.73609336480919,-1.00869174677624));
#14935=CARTESIAN_POINT('Ctrl Pts',(90.3498698986825,-1.76480709242939,-0.943133950083889));
#14936=CARTESIAN_POINT('Ctrl Pts',(90.3498698986825,-1.78957581065152,-0.87622659827583));
#14937=CARTESIAN_POINT('Ctrl Pts',(90.3498698986825,-1.79745850834223,-0.854933190080087));
#14938=CARTESIAN_POINT('Ctrl Pts',(90.3498698986825,-1.80494126151048,-0.833502987156274));
#14939=CARTESIAN_POINT('Ctrl Pts',(90.3498698986825,-1.81201458800381,-0.811941804694479));
#14940=CARTESIAN_POINT('Ctrl Pts',(90.3498698986825,-1.83480258848545,-0.742478556138484));
#14941=CARTESIAN_POINT('Ctrl Pts',(90.3498698986825,-1.85334501760416,-0.671655559771788));
#14942=CARTESIAN_POINT('Ctrl Pts',(90.3498698986825,-1.86769676550017,-0.59983269942607));
#14943=CARTESIAN_POINT('Ctrl Pts',(90.3498698986825,-1.88119220525599,-0.532295205602301));
#14944=CARTESIAN_POINT('Ctrl Pts',(90.3498698986825,-1.89098144653587,-0.463872822082176));
#14945=CARTESIAN_POINT('Ctrl Pts',(90.3498698986825,-1.89706925925139,-0.394874641297999));
#14946=CARTESIAN_POINT('Ctrl Pts',(90.3498698986825,-1.89846100872211,-0.379100801649089));
#14947=CARTESIAN_POINT('Ctrl Pts',(90.3498698986825,-1.89965930467989,-0.363292543085898));
#14948=CARTESIAN_POINT('Ctrl Pts',(90.3498698986825,-1.90066249818027,-0.347482308863445));
#14949=CARTESIAN_POINT('Ctrl Pts',(90.3498698986825,-1.90518355320199,-0.276230911402284));
#14950=CARTESIAN_POINT('Ctrl Pts',(90.3498698986825,-1.90575774275495,-0.204834546578483));
#14951=CARTESIAN_POINT('Ctrl Pts',(90.3498698986825,-1.90246416417068,-0.13362783011485));
#14952=CARTESIAN_POINT('Ctrl Pts',(90.3498698986825,-1.89918981651357,-0.0628368836537749));
#14953=CARTESIAN_POINT('Ctrl Pts',(90.3498698986825,-1.89209235575437,0.00776763404536897));
#14954=CARTESIAN_POINT('Ctrl Pts',(90.3498698986825,-1.88120052059324,0.0778439104102741));
#14955=CARTESIAN_POINT('Ctrl Pts',(90.3498698986825,-1.87040101395053,0.147326160270228));
#14956=CARTESIAN_POINT('Ctrl Pts',(90.3498698986825,-1.85587082136304,0.216290003110817));
#14957=CARTESIAN_POINT('Ctrl Pts',(90.3498698986825,-1.83759523778481,0.284375112098316));
#14958=CARTESIAN_POINT('Ctrl Pts',(90.3498698986825,-1.83323021278473,0.300636874771509));
#14959=CARTESIAN_POINT('Ctrl Pts',(90.3498698986825,-1.82865134630036,0.316848351257569));
#14960=CARTESIAN_POINT('Ctrl Pts',(90.3498698986825,-1.82385810846295,0.333004312157768));
#14961=CARTESIAN_POINT('Ctrl Pts',(90.3498698986825,-1.81957084053952,0.347454864224923));
#14962=CARTESIAN_POINT('Ctrl Pts',(90.3498698986825,-1.81511076839976,0.361864640445972));
#14963=CARTESIAN_POINT('Ctrl Pts',(90.3498698986825,-1.81048601405767,0.376204364629576));
#14964=CARTESIAN_POINT('Ctrl Pts',(90.3498698986825,-1.78940703160402,0.441562818743621));
#14965=CARTESIAN_POINT('Ctrl Pts',(90.3498698986825,-1.76488237508185,0.505569487086397));
#14966=CARTESIAN_POINT('Ctrl Pts',(90.3498698986825,-1.73694698977818,0.567913160502579));
#14967=CARTESIAN_POINT('Ctrl Pts',(90.3498698986825,-1.70948750852825,0.629194754173614));
#14968=CARTESIAN_POINT('Ctrl Pts',(90.3498698986825,-1.67873208505158,0.68887029218068));
#14969=CARTESIAN_POINT('Ctrl Pts',(90.3498698986825,-1.64467466487717,0.746613674873613));
#14970=CARTESIAN_POINT('Ctrl Pts',(90.3498698986825,-1.61171139288394,0.802501960591362));
#14971=CARTESIAN_POINT('Ctrl Pts',(90.3498698986825,-1.57565443941957,0.856580748546144));
#14972=CARTESIAN_POINT('Ctrl Pts',(90.3498698986825,-1.53646769662718,0.908516538747599));
#14973=CARTESIAN_POINT('Ctrl Pts',(90.3498698986825,-1.52109669050737,0.928888360750091));
#14974=CARTESIAN_POINT('Ctrl Pts',(90.3498698986825,-1.50524382897348,0.948930000897413));
#14975=CARTESIAN_POINT('Ctrl Pts',(90.3498698986825,-1.48890580190332,0.968619417293828));
#14976=CARTESIAN_POINT('Ctrl Pts',(90.1012771668264,-1.84931296668343,1.20406753850538));
#14977=CARTESIAN_POINT('Ctrl Pts',(90.1410089197541,-2.25011488217789,0.588520614799742));
#14978=CARTESIAN_POINT('Ctrl Pts',(90.2204575780214,-2.38112656801824,-1.0636724344526));
#14979=CARTESIAN_POINT('Ctrl Pts',(90.3396231416286,-0.39278540449122,-2.58069915842425));
#14980=CARTESIAN_POINT('Ctrl Pts',(90.4587738576477,1.95479315758241,-1.7268362990989));
#14981=CARTESIAN_POINT('Ctrl Pts',(90.5779245736668,2.51126427646298,0.706567951536284));
#14982=CARTESIAN_POINT('Ctrl Pts',(90.697075289686,0.76642661853108,2.49393221007964));
#14983=CARTESIAN_POINT('Ctrl Pts',(90.8162260057051,-1.68068835309601,1.9952419118154));
#14984=CARTESIAN_POINT('Ctrl Pts',(90.9353767217243,-2.58771188198714,-0.331445932145255));
#14985=CARTESIAN_POINT('Ctrl Pts',(91.0545274377435,-1.12345126024935,-2.35459120720293));
#14986=CARTESIAN_POINT('Ctrl Pts',(91.1736781537624,1.37028833406634,-2.21999495043472));
#14987=CARTESIAN_POINT('Ctrl Pts',(91.2928288697817,2.60835478940657,-0.051132071917531));
#14988=CARTESIAN_POINT('Ctrl Pts',(91.4119795858008,1.45623058597522,2.16460903716915));
#14989=CARTESIAN_POINT('Ctrl Pts',(91.5311303018199,-1.03032282425427,2.39677979879221));
#14990=CARTESIAN_POINT('Ctrl Pts',(91.6502810178392,-2.57273105870856,0.432645731205606));
#14991=CARTESIAN_POINT('Ctrl Pts',(91.7694317338581,-1.75759399985632,-1.92795002038761));
#14992=CARTESIAN_POINT('Ctrl Pts',(91.8885824498775,0.668129948444457,-2.52185007357365));
#14993=CARTESIAN_POINT('Ctrl Pts',(92.0077331658964,2.48160708881929,-0.804830990088789));
#14994=CARTESIAN_POINT('Ctrl Pts',(92.1268838819157,2.02104135775696,1.64970253573836));
#14995=CARTESIAN_POINT('Ctrl Pts',(92.2460345979347,-0.291523684063095,
2.59251620548281));
#14996=CARTESIAN_POINT('Ctrl Pts',(92.3651853139538,-2.33694839666172,1.15965455820404));
#14997=CARTESIAN_POINT('Ctrl Pts',(92.4843360299731,-2.24088954394834,-1.33586696065266));
#14998=CARTESIAN_POINT('Ctrl Pts',(92.6034867459922,-0.0913715189856824,
-2.60725482022871));
#14999=CARTESIAN_POINT('Ctrl Pts',(92.7226374620113,2.141875615255,-1.48946142052775));
#15000=CARTESIAN_POINT('Ctrl Pts',(92.8417881780305,2.41239587446518,0.993213277893959));
#15001=CARTESIAN_POINT('Ctrl Pts',(92.9609388940497,0.472295600424488,2.56574810393475));
#15002=CARTESIAN_POINT('Ctrl Pts',(93.0800896100686,-1.90059697085994,1.78713671113314));
#15003=CARTESIAN_POINT('Ctrl Pts',(93.199240326088,-2.53186051096024,-0.629133389884245));
#15004=CARTESIAN_POINT('Ctrl Pts',(93.318391042107,-0.843031029634389,-2.46889148241641));
#15005=CARTESIAN_POINT('Ctrl Pts',(93.4375417581261,1.61831747486931,-2.04625878612023));
#15006=CARTESIAN_POINT('Ctrl Pts',(93.5566924741453,2.59670628878377,0.251481448464151));
#15007=CARTESIAN_POINT('Ctrl Pts',(93.6758431901645,1.19558007283248,2.31877440872209));
#15008=CARTESIAN_POINT('Ctrl Pts',(93.7949939061835,-1.30112663483962,2.26123770295275));
#15009=CARTESIAN_POINT('Ctrl Pts',(93.9141446222028,-2.60553431480175,0.131595605998399));
#15010=CARTESIAN_POINT('Ctrl Pts',(94.0332953382218,-1.52233732430562,-2.11863530135582));
#15011=CARTESIAN_POINT('Ctrl Pts',(94.152446054241,0.95586708746203,-2.42743580352548));
#15012=CARTESIAN_POINT('Ctrl Pts',(94.2715967702601,2.55815414538899,-0.511833798764109));
#15013=CARTESIAN_POINT('Ctrl Pts',(94.3907474862793,1.81625377481591,1.87279168478371));
#15014=CARTESIAN_POINT('Ctrl Pts',(94.5098982022984,-0.589986984925512,
2.54126775975048));
#15015=CARTESIAN_POINT('Ctrl Pts',(94.6290489183177,-2.45558789482286,0.881030396710455));
#15016=CARTESIAN_POINT('Ctrl Pts',(94.7481996343365,-2.07098887716839,-1.58654704934119));
#15017=CARTESIAN_POINT('Ctrl Pts',(94.8673503503559,0.211379318771256,-2.60027791836263));
#15018=CARTESIAN_POINT('Ctrl Pts',(94.9865010663749,2.30004818560611,-1.23122086280996));
#15019=CARTESIAN_POINT('Ctrl Pts',(95.1056517823941,2.28104732840938,1.26607644109069));
#15020=CARTESIAN_POINT('Ctrl Pts',(95.2248024984132,0.171788352596476,2.60319327577509));
#15021=CARTESIAN_POINT('Ctrl Pts',(95.3439532144324,-2.09489041640805,1.55485067204866));
#15022=CARTESIAN_POINT('Ctrl Pts',(95.4631039304515,-2.44189761789554,-0.918293249917765));
#15023=CARTESIAN_POINT('Ctrl Pts',(95.5822546464707,-0.551250099524635,
-2.54995094009719));
#15024=CARTESIAN_POINT('Ctrl Pts',(95.7014053624896,1.84454037733229,-1.84493828230628));
#15025=CARTESIAN_POINT('Ctrl Pts',(95.8205560785091,2.55006978384011,0.550700069615015));
#15026=CARTESIAN_POINT('Ctrl Pts',(95.939706794528,0.918819938851015,2.44169948787694));
#15027=CARTESIAN_POINT('Ctrl Pts',(96.0588575105472,-1.55439877403927,2.09522574449468));
#15028=CARTESIAN_POINT('Ctrl Pts',(96.1780082265663,-2.60323026947166,-0.171226847295238));
#15029=CARTESIAN_POINT('Ctrl Pts',(96.2971589425855,-1.26656842698869,-2.28077418629858));
#15030=CARTESIAN_POINT('Ctrl Pts',(96.4163096586046,1.23072472038826,-2.30031370290016));
#15031=CARTESIAN_POINT('Ctrl Pts',(96.5354603746238,2.6002322639617,-0.211940186326234));
#15032=CARTESIAN_POINT('Ctrl Pts',(96.6546110906428,1.58699371878083,2.07064661535818));
#15033=CARTESIAN_POINT('Ctrl Pts',(96.7737618066621,-0.880500712968156,
2.45577787341633));
#15034=CARTESIAN_POINT('Ctrl Pts',(96.8929125226811,-2.54114044213503,0.590535115362907));
#15035=CARTESIAN_POINT('Ctrl Pts',(97.0120632387003,-1.87318340193992,-1.81584977680931));
#15036=CARTESIAN_POINT('Ctrl Pts',(97.1312139547194,0.511282000374004,-2.55826448690676));
#15037=CARTESIAN_POINT('Ctrl Pts',(97.2503646707386,2.42722956925394,-0.956390656252166));
#15038=CARTESIAN_POINT('Ctrl Pts',(97.3695153867577,2.11896361589558,1.52188030555377));
#15039=CARTESIAN_POINT('Ctrl Pts',(97.4886661027769,-0.131033596758635,
2.60556263857647));
#15040=CARTESIAN_POINT('Ctrl Pts',(97.607816818796,-2.26095700091368,1.30161434785459));
#15041=CARTESIAN_POINT('Ctrl Pts',(97.7269675348151,-2.31903223828938,-1.19507989366364));
#15042=CARTESIAN_POINT('Ctrl Pts',(97.8461182508343,-0.252041544049245,
-2.59665198133307));
#15043=CARTESIAN_POINT('Ctrl Pts',(97.9652689668533,2.04590967080785,-1.61875881577068));
#15044=CARTESIAN_POINT('Ctrl Pts',(98.0844196828726,2.46907326691131,0.842498489996876));
#15045=CARTESIAN_POINT('Ctrl Pts',(98.2035703988916,0.629679485185892,2.53172472437204));
#15046=CARTESIAN_POINT('Ctrl Pts',(98.3227211149109,-1.78672670610972,1.9009824575361));
#15047=CARTESIAN_POINT('Ctrl Pts',(98.4418718309298,-2.5658499372617,-0.471742265797349));
#15048=CARTESIAN_POINT('Ctrl Pts',(98.5610225469492,-0.993733561394519,
-2.41218138425575));
#15049=CARTESIAN_POINT('Ctrl Pts',(98.6801732629682,1.48899930931111,-2.14219723795793));
#15050=CARTESIAN_POINT('Ctrl Pts',(98.7993239789874,2.60727462778386,0.0908099360674505));
#15051=CARTESIAN_POINT('Ctrl Pts',(98.9184746950065,1.33634996509571,2.24059976275692));
#15052=CARTESIAN_POINT('Ctrl Pts',(99.0376254110257,-1.15914982504648,2.33720163580698));
#15053=CARTESIAN_POINT('Ctrl Pts',(99.1567761270448,-2.59245452524983,0.292076583639263));
#15054=CARTESIAN_POINT('Ctrl Pts',(99.2759268430639,-1.65013591906561,-2.02067294410637));
#15055=CARTESIAN_POINT('Ctrl Pts',(99.3950775590831,0.804290694920273,-2.4818055857093));
#15056=CARTESIAN_POINT('Ctrl Pts',(99.5142282751021,2.52171586070367,-0.668624190400465));
#15057=CARTESIAN_POINT('Ctrl Pts',(99.6333789911213,1.9283092486174,1.75707912986123));
#15058=CARTESIAN_POINT('Ctrl Pts',(99.7525297071405,-0.432051285021002,
2.57302143737229));
#15059=CARTESIAN_POINT('Ctrl Pts',(99.8716804231596,-2.39663622909211,1.0304471465245));
#15060=CARTESIAN_POINT('Ctrl Pts',(99.9908311391787,-2.16476570723772,-1.45498086777256));
#15061=CARTESIAN_POINT('Ctrl Pts',(100.109981855198,0.0502481845584496,
-2.60993556246539));
#15062=CARTESIAN_POINT('Ctrl Pts',(100.229132571217,2.22042935661311,-1.36750819077076));
#15063=CARTESIAN_POINT('Ctrl Pts',(100.308566381897,2.30790711033604,0.287109651903352));
#15064=CARTESIAN_POINT('Ctrl Pts',(100.348283287236,1.99185752827467,0.949863530723621));
#15065=CARTESIAN_POINT('Ctrl Pts',(90.1847484975003,-1.72815398363866,1.12518224374417));
#15066=CARTESIAN_POINT('Ctrl Pts',(90.224480250428,-2.10269709202011,0.54996329082341));
#15067=CARTESIAN_POINT('Ctrl Pts',(90.3039289086954,-2.22512545913109,-0.993985219377189));
#15068=CARTESIAN_POINT('Ctrl Pts',(90.4230944723026,-0.367051804489291,
-2.41162291702421));
#15069=CARTESIAN_POINT('Ctrl Pts',(90.5422451883216,1.82672356887439,-1.61370145732095));
#15070=CARTESIAN_POINT('Ctrl Pts',(90.6613959043407,2.34673710806346,0.660276676883258));
#15071=CARTESIAN_POINT('Ctrl Pts',(90.78054662036,0.71621366304295,2.33054056366851));
#15072=CARTESIAN_POINT('Ctrl Pts',(90.899697336379,-1.57057692504417,1.86452229576392));
#15073=CARTESIAN_POINT('Ctrl Pts',(91.0188480523982,-2.41817619728542,-0.309731028937152));
#15074=CARTESIAN_POINT('Ctrl Pts',(91.1379987684174,-1.04984759518864,-2.20032858032993));
#15075=CARTESIAN_POINT('Ctrl Pts',(91.2571494844365,1.28051297206727,-2.07455048786676));
#15076=CARTESIAN_POINT('Ctrl Pts',(91.3763002004557,2.43746667073877,-0.0477821198293046));
#15077=CARTESIAN_POINT('Ctrl Pts',(91.4954509164748,1.36082465952898,2.0227932199669));
#15078=CARTESIAN_POINT('Ctrl Pts',(91.6146016324938,-0.962820531325284,
2.23975315796098));
#15079=CARTESIAN_POINT('Ctrl Pts',(91.733752348513,-2.40417685272153,0.404300655084951));
#15080=CARTESIAN_POINT('Ctrl Pts',(91.8529030645321,-1.64244404662254,-1.80163907787028));
#15081=CARTESIAN_POINT('Ctrl Pts',(91.9720537805513,0.624356965421232,-2.35662936955536));
#15082=CARTESIAN_POINT('Ctrl Pts',(92.0912044965705,2.31902293101863,-0.752101946363442));
#15083=CARTESIAN_POINT('Ctrl Pts',(92.2103552125894,1.88863147364933,1.54162116435486));
#15084=CARTESIAN_POINT('Ctrl Pts',(92.3295059286088,-0.272424313793784,
2.42266576229539));
#15085=CARTESIAN_POINT('Ctrl Pts',(92.4486566446278,-2.18384165038965,1.08367900972386));
#15086=CARTESIAN_POINT('Ctrl Pts',(92.567807360647,-2.09407615803056,-1.24834673808803));
#15087=CARTESIAN_POINT('Ctrl Pts',(92.686958076666,-0.0853852524537151,
-2.43643876678157));
#15088=CARTESIAN_POINT('Ctrl Pts',(92.8061087926853,2.00154919348222,-1.39187835360143));
#15089=CARTESIAN_POINT('Ctrl Pts',(92.9252595087044,2.2543461359313,0.928142241858348));
#15090=CARTESIAN_POINT('Ctrl Pts',(93.0444102247236,0.441352836449495,2.39765139092715));
#15091=CARTESIAN_POINT('Ctrl Pts',(93.1635609407427,-1.7760780817828,1.67005124729668));
#15092=CARTESIAN_POINT('Ctrl Pts',(93.2827116567617,-2.36598396640256,-0.587915292628069));
#15093=CARTESIAN_POINT('Ctrl Pts',(93.401862372781,-0.787799284621054,-2.30714039612304));
#15094=CARTESIAN_POINT('Ctrl Pts',(93.5210130888001,1.51229231686137,-1.91219676522963));
#15095=CARTESIAN_POINT('Ctrl Pts',(93.6401638048192,2.42658132947023,0.235005472196508));
#15096=CARTESIAN_POINT('Ctrl Pts',(93.7593145208384,1.11725084009434,2.16685834349552));
#15097=CARTESIAN_POINT('Ctrl Pts',(93.8784652368574,-1.21588244809045,2.11309119370958));
#15098=CARTESIAN_POINT('Ctrl Pts',(93.9976159528767,-2.43483098142503,0.122974031347059));
#15099=CARTESIAN_POINT('Ctrl Pts',(94.1167666688958,-1.42260037042766,-1.9798314843819));
#15100=CARTESIAN_POINT('Ctrl Pts',(94.2359173849148,0.893242812215344,-2.26840071392186));
#15101=CARTESIAN_POINT('Ctrl Pts',(94.3550681009339,2.39055495568398,-0.478300663127559));
#15102=CARTESIAN_POINT('Ctrl Pts',(94.4742188169533,1.69726068696523,1.75009447772847));
#15103=CARTESIAN_POINT('Ctrl Pts',(94.5933695329723,-0.551333590723985,
2.37477489296004));
#15104=CARTESIAN_POINT('Ctrl Pts',(94.7125202489916,-2.29470840202001,0.823309097600963));
#15105=CARTESIAN_POINT('Ctrl Pts',(94.8316709650105,-1.93530664772684,-1.48260335213368));
#15106=CARTESIAN_POINT('Ctrl Pts',(94.9508216810298,0.197530660507136,-2.4299189613346));
#15107=CARTESIAN_POINT('Ctrl Pts',(95.0699723970489,2.14935898148411,-1.15055659974088));
#15108=CARTESIAN_POINT('Ctrl Pts',(95.189123113068,2.13160297822848,1.18312859136324));
#15109=CARTESIAN_POINT('Ctrl Pts',(95.3082738290871,0.16053352311411,2.43264331714503));
#15110=CARTESIAN_POINT('Ctrl Pts',(95.4274245451062,-1.95764226154465,1.45298358432161));
#15111=CARTESIAN_POINT('Ctrl Pts',(95.5465752611255,-2.281915052795,-0.858130649913704));
#15112=CARTESIAN_POINT('Ctrl Pts',(95.6657259771446,-0.515134578428419,
-2.38288918890517));
#15113=CARTESIAN_POINT('Ctrl Pts',(95.7848766931636,1.72369407368938,-1.72406590965131));
#15114=CARTESIAN_POINT('Ctrl Pts',(95.9040274091828,2.38300024652033,0.514620584098359));
#15115=CARTESIAN_POINT('Ctrl Pts',(96.023178125202,0.858622832467166,2.28172990339787));
#15116=CARTESIAN_POINT('Ctrl Pts',(96.1423288412211,-1.45256129271431,1.95795562038611));
#15117=CARTESIAN_POINT('Ctrl Pts',(96.2614795572402,-2.43267788717467,-0.16000880521043));
#15118=CARTESIAN_POINT('Ctrl Pts',(96.3806302732593,-1.18358834447416,-2.13134773120684));
#15119=CARTESIAN_POINT('Ctrl Pts',(96.4997809892786,1.15009296242373,-2.14960710323403));
#15120=CARTESIAN_POINT('Ctrl Pts',(96.6189317052976,2.42987629801246,-0.198054782446931));
#15121=CARTESIAN_POINT('Ctrl Pts',(96.7380824213169,1.48302075772449,1.93498680942938));
#15122=CARTESIAN_POINT('Ctrl Pts',(96.8572331373359,-0.822814116445383,
2.2948859340381));
#15123=CARTESIAN_POINT('Ctrl Pts',(96.9763838533551,-2.37465591664382,0.551845810027022));
#15124=CARTESIAN_POINT('Ctrl Pts',(97.0955345693742,-1.75046053127167,-1.69688315715983));
#15125=CARTESIAN_POINT('Ctrl Pts',(97.2146852853935,0.4777850161802,-2.39065806810298));
#15126=CARTESIAN_POINT('Ctrl Pts',(97.3338360014124,2.26820799122736,-0.893732079043964));
#15127=CARTESIAN_POINT('Ctrl Pts',(97.4529867174316,1.98013828917371,1.4221732935668));
#15128=CARTESIAN_POINT('Ctrl Pts',(97.5721374334508,-0.122448842520727,
2.43485744954859));
#15129=CARTESIAN_POINT('Ctrl Pts',(97.6912881494699,-2.11282888205345,1.21633820825914));
#15130=CARTESIAN_POINT('Ctrl Pts',(97.8104388654891,-2.16709928118526,-1.11678343050024));
#15131=CARTESIAN_POINT('Ctrl Pts',(97.9295895815082,-0.235528872742544,
-2.42653058000869));
#15132=CARTESIAN_POINT('Ctrl Pts',(98.0487402975273,1.91187052244181,-1.51270474301667));
#15133=CARTESIAN_POINT('Ctrl Pts',(98.1678910135465,2.30731027088445,0.787301634676153));
#15134=CARTESIAN_POINT('Ctrl Pts',(98.2870417295656,0.588425610128645,2.36585707596402));
#15135=CARTESIAN_POINT('Ctrl Pts',(98.4061924455848,-1.66966810402821,1.77643831304004));
#15136=CARTESIAN_POINT('Ctrl Pts',(98.5253431616039,-2.39774655257518,-0.440835753912708));
#15137=CARTESIAN_POINT('Ctrl Pts',(98.644493877623,-0.928628438635352,-2.25414569819225));
#15138=CARTESIAN_POINT('Ctrl Pts',(98.7636445936422,1.39144651791202,-2.0018497448574));
#15139=CARTESIAN_POINT('Ctrl Pts',(98.8827953096614,2.43645727663141,0.0848604620181749));
#15140=CARTESIAN_POINT('Ctrl Pts',(99.0019460256804,1.24879809817007,2.09380536204883));
#15141=CARTESIAN_POINT('Ctrl Pts',(99.1210967416997,-1.08320734449868,2.18407829840195));
#15142=CARTESIAN_POINT('Ctrl Pts',(99.2402474577186,-2.42260812308438,0.272940989782257));
#15143=CARTESIAN_POINT('Ctrl Pts',(99.359398173738,-1.54202615428187,-1.8882871968669));
#15144=CARTESIAN_POINT('Ctrl Pts',(99.4785488897569,0.751597048996372,-2.31920842325136));
#15145=CARTESIAN_POINT('Ctrl Pts',(99.5976996057762,2.35650394973185,-0.624818826782988));
#15146=CARTESIAN_POINT('Ctrl Pts',(99.7168503217953,1.80197477102092,1.64196290868155));
#15147=CARTESIAN_POINT('Ctrl Pts',(99.8360010378144,-0.403745154442039,
2.40444820703176));
#15148=CARTESIAN_POINT('Ctrl Pts',(99.9551517538334,-2.23961899432637,0.962936708538316));
#15149=CARTESIAN_POINT('Ctrl Pts',(100.074302469853,-2.02293962569051,-1.35965681745507));
#15150=CARTESIAN_POINT('Ctrl Pts',(100.193453185872,0.0469561409451712,
-2.43894387838727));
#15151=CARTESIAN_POINT('Ctrl Pts',(100.312603901891,2.07495643363217,-1.27791497172988));
#15152=CARTESIAN_POINT('Ctrl Pts',(100.392037712571,2.15670302347367,0.268299469920303));
#15153=CARTESIAN_POINT('Ctrl Pts',(100.43175461791,1.86135964238754,0.887632582535241));
#15154=CARTESIAN_POINT('Ctrl Pts',(90.2682198281743,-1.60699500059389,1.04629694898296));
#15155=CARTESIAN_POINT('Ctrl Pts',(90.3079515811019,-1.95527930186235,0.511405966847078));
#15156=CARTESIAN_POINT('Ctrl Pts',(90.3874002393695,-2.06912435024394,-0.924298004301774));
#15157=CARTESIAN_POINT('Ctrl Pts',(90.5065658029763,-0.341318204487364,
-2.24254667562417));
#15158=CARTESIAN_POINT('Ctrl Pts',(90.6257165189957,1.69865398016637,-1.50056661554299));
#15159=CARTESIAN_POINT('Ctrl Pts',(90.7448672350146,2.18220993966394,0.613985402230233));
#15160=CARTESIAN_POINT('Ctrl Pts',(90.8640179510338,0.666000707554823,2.16714891725738));
#15161=CARTESIAN_POINT('Ctrl Pts',(90.983168667053,-1.46046549699233,1.73380267971244));
#15162=CARTESIAN_POINT('Ctrl Pts',(91.1023193830721,-2.2486405125837,-0.288016125729047));
#15163=CARTESIAN_POINT('Ctrl Pts',(91.2214700990913,-0.976243930127919,
-2.04606595345694));
#15164=CARTESIAN_POINT('Ctrl Pts',(91.3406208151105,1.1907376100682,-1.92910602529881));
#15165=CARTESIAN_POINT('Ctrl Pts',(91.4597715311294,2.26657855207099,-0.0444321677410789));
#15166=CARTESIAN_POINT('Ctrl Pts',(91.5789222471488,1.26541873308275,1.88097740276464));
#15167=CARTESIAN_POINT('Ctrl Pts',(91.6980729631677,-0.89531823839629,2.08272651712975));
#15168=CARTESIAN_POINT('Ctrl Pts',(91.817223679187,-2.2356226467345,0.375955578964296));
#15169=CARTESIAN_POINT('Ctrl Pts',(91.9363743952059,-1.52729409338877,-1.67532813535295));
#15170=CARTESIAN_POINT('Ctrl Pts',(92.0555251112253,0.580583982398003,-2.19140866553707));
#15171=CARTESIAN_POINT('Ctrl Pts',(92.1746758272442,2.15643877321799,-0.699372902638098));
#15172=CARTESIAN_POINT('Ctrl Pts',(92.2938265432635,1.75622158954171,1.43353979297137));
#15173=CARTESIAN_POINT('Ctrl Pts',(92.4129772592825,-0.253324943524471,
2.25281531910798));
#15174=CARTESIAN_POINT('Ctrl Pts',(92.5321279753018,-2.03073490411758,1.0077034612437));
#15175=CARTESIAN_POINT('Ctrl Pts',(92.6512786913209,-1.94726277211276,-1.16082651552341));
#15176=CARTESIAN_POINT('Ctrl Pts',(92.77042940734,-0.0793989859217509,-2.26562271333442));
#15177=CARTESIAN_POINT('Ctrl Pts',(92.8895801233591,1.86122277170944,-1.2942952866751));
#15178=CARTESIAN_POINT('Ctrl Pts',(93.0087308393784,2.09629639739743,0.863071205822738));
#15179=CARTESIAN_POINT('Ctrl Pts',(93.1278815553974,0.410410072474505,2.22955467791957));
#15180=CARTESIAN_POINT('Ctrl Pts',(93.2470322714165,-1.65155919270567,1.55296578346024));
#15181=CARTESIAN_POINT('Ctrl Pts',(93.3661829874357,-2.20010742184487,-0.546697195371894));
#15182=CARTESIAN_POINT('Ctrl Pts',(93.4853337034548,-0.732567539607717,
-2.14538930982965));
#15183=CARTESIAN_POINT('Ctrl Pts',(93.6044844194739,1.40626715885344,-1.77813474433903));
#15184=CARTESIAN_POINT('Ctrl Pts',(93.7236351354933,2.25645637015669,0.218529495928864));
#15185=CARTESIAN_POINT('Ctrl Pts',(93.8427858515121,1.0389216073562,2.01494227826896));
#15186=CARTESIAN_POINT('Ctrl Pts',(93.9619365675316,-1.13063826134128,1.96494468446641));
#15187=CARTESIAN_POINT('Ctrl Pts',(94.0810872835504,-2.2641276480483,0.11435245669572));
#15188=CARTESIAN_POINT('Ctrl Pts',(94.2002379995699,-1.32286341654972,-1.84102766740798));
#15189=CARTESIAN_POINT('Ctrl Pts',(94.3193887155888,0.830618536968657,-2.10936562431824));
#15190=CARTESIAN_POINT('Ctrl Pts',(94.4385394316082,2.22295576597898,-0.444767527491008));
#15191=CARTESIAN_POINT('Ctrl Pts',(94.5576901476269,1.57826759911456,1.62739727067323));
#15192=CARTESIAN_POINT('Ctrl Pts',(94.6768408636463,-0.512680196522462,
2.20828202616961));
#15193=CARTESIAN_POINT('Ctrl Pts',(94.7959915796653,-2.13382890921714,0.76558779849147));
#15194=CARTESIAN_POINT('Ctrl Pts',(94.9151422956845,-1.79962441828529,-1.37865965492618));
#15195=CARTESIAN_POINT('Ctrl Pts',(95.0342930117036,0.183682002243022,-2.25956000430656));
#15196=CARTESIAN_POINT('Ctrl Pts',(95.1534437277228,1.99866977736211,-1.06989233667182));
#15197=CARTESIAN_POINT('Ctrl Pts',(95.272594443742,1.9821586280476,1.1001807416358));
#15198=CARTESIAN_POINT('Ctrl Pts',(95.3917451597611,0.149278693631744,2.26209335851495));
#15199=CARTESIAN_POINT('Ctrl Pts',(95.5108958757802,-1.82039410668127,1.35111649659456));
#15200=CARTESIAN_POINT('Ctrl Pts',(95.6300465917994,-2.12193248769446,-0.797968049909645));
#15201=CARTESIAN_POINT('Ctrl Pts',(95.7491973078186,-0.479019057332203,
-2.21582743771315));
#15202=CARTESIAN_POINT('Ctrl Pts',(95.8683480238375,1.60284777004647,-1.60319353699634));
#15203=CARTESIAN_POINT('Ctrl Pts',(95.9874987398567,2.21593070920054,0.478541098581703));
#15204=CARTESIAN_POINT('Ctrl Pts',(96.1066494558759,0.798425726083314,2.12176031891879));
#15205=CARTESIAN_POINT('Ctrl Pts',(96.2258001718951,-1.35072381138935,1.82068549627755));
#15206=CARTESIAN_POINT('Ctrl Pts',(96.3449508879141,-2.26212550487769,-0.148790763125627));
#15207=CARTESIAN_POINT('Ctrl Pts',(96.4641016039334,-1.10060826195961,-1.98192127611509));
#15208=CARTESIAN_POINT('Ctrl Pts',(96.5832523199524,1.0694612044592,-1.99890050356789));
#15209=CARTESIAN_POINT('Ctrl Pts',(96.7024030359715,2.25952033206322,-0.184169378567629));
#15210=CARTESIAN_POINT('Ctrl Pts',(96.8215537519909,1.37904779666815,1.79932700350057));
#15211=CARTESIAN_POINT('Ctrl Pts',(96.9407044680099,-0.765127519922608,
2.13399399465988));
#15212=CARTESIAN_POINT('Ctrl Pts',(97.0598551840291,-2.20817139115261,0.513156504691141));
#15213=CARTESIAN_POINT('Ctrl Pts',(97.1790059000482,-1.62773766060341,-1.57791653751034));
#15214=CARTESIAN_POINT('Ctrl Pts',(97.2981566160672,0.444288031986397,-2.22305164929921));
#15215=CARTESIAN_POINT('Ctrl Pts',(97.4173073320864,2.10918641320078,-0.831073501835764));
#15216=CARTESIAN_POINT('Ctrl Pts',(97.5364580481055,1.84131296245185,1.32246628157985));
#15217=CARTESIAN_POINT('Ctrl Pts',(97.6556087641247,-0.113864088282822,
2.26415226052072));
#15218=CARTESIAN_POINT('Ctrl Pts',(97.774759480144,-1.96470076319321,1.13106206866369));
#15219=CARTESIAN_POINT('Ctrl Pts',(97.8939101961629,-2.01516632408114,-1.03848696733685));
#15220=CARTESIAN_POINT('Ctrl Pts',(98.0130609121822,-0.219016201435841,
-2.25640917868432));
#15221=CARTESIAN_POINT('Ctrl Pts',(98.1322116282013,1.77783137407576,-1.40665067026268));
#15222=CARTESIAN_POINT('Ctrl Pts',(98.2513623442205,2.1455472748576,0.732104779355433));
#15223=CARTESIAN_POINT('Ctrl Pts',(98.3705130602396,0.547171735071399,2.19998942755601));
#15224=CARTESIAN_POINT('Ctrl Pts',(98.4896637762586,-1.55260950194669,1.65189416854399));
#15225=CARTESIAN_POINT('Ctrl Pts',(98.6088144922779,-2.22964316788868,-0.409929242028069));
#15226=CARTESIAN_POINT('Ctrl Pts',(98.727965208297,-0.863523315876183,-2.09611001212873));
#15227=CARTESIAN_POINT('Ctrl Pts',(98.8471159243161,1.29389372651294,-1.86150225175686));
#15228=CARTESIAN_POINT('Ctrl Pts',(98.9662666403352,2.26563992547896,0.0789109879689021));
#15229=CARTESIAN_POINT('Ctrl Pts',(99.0854173563544,1.16124623124442,1.94701096134075));
#15230=CARTESIAN_POINT('Ctrl Pts',(99.2045680723735,-1.00726486395089,2.03095496099691));
#15231=CARTESIAN_POINT('Ctrl Pts',(99.3237187883926,-2.25276172091894,0.253805395925249));
#15232=CARTESIAN_POINT('Ctrl Pts',(99.4428695044117,-1.43391638949813,-1.75590144962745));
#15233=CARTESIAN_POINT('Ctrl Pts',(99.5620202204309,0.69890340307247,-2.15661126079343));
#15234=CARTESIAN_POINT('Ctrl Pts',(99.68117093645,2.19129203876002,-0.581013463165512));
#15235=CARTESIAN_POINT('Ctrl Pts',(99.8003216524693,1.67564029342444,1.52684668750188));
#15236=CARTESIAN_POINT('Ctrl Pts',(99.9194723684883,-0.375439023863076,
2.23587497669124));
#15237=CARTESIAN_POINT('Ctrl Pts',(100.038623084508,-2.08260175956064,0.895426270552136));
#15238=CARTESIAN_POINT('Ctrl Pts',(100.157773800527,-1.88111354414331,-1.26433276713758));
#15239=CARTESIAN_POINT('Ctrl Pts',(100.276924516546,0.0436640973318916,
-2.26795219430915));
#15240=CARTESIAN_POINT('Ctrl Pts',(100.396075232565,1.92948351065122,-1.18832175268901));
#15241=CARTESIAN_POINT('Ctrl Pts',(100.475509043245,2.00549893661128,0.249489287937253));
#15242=CARTESIAN_POINT('Ctrl Pts',(100.515225948584,1.73086175650041,0.82540163434686));
#15243=CARTESIAN_POINT('Ctrl Pts',(90.3516911588482,-1.48583601754912,0.967411654221745));
#15244=CARTESIAN_POINT('Ctrl Pts',(90.3914229117759,-1.80786151170457,0.472848642870747));
#15245=CARTESIAN_POINT('Ctrl Pts',(90.4708715700433,-1.91312324135679,-0.854610789226363));
#15246=CARTESIAN_POINT('Ctrl Pts',(90.5900371336504,-0.315584604485434,
-2.07347043422413));
#15247=CARTESIAN_POINT('Ctrl Pts',(90.7091878496695,1.57058439145835,-1.38743177376504));
#15248=CARTESIAN_POINT('Ctrl Pts',(90.8283385656886,2.01768277126442,0.567694127577208));
#15249=CARTESIAN_POINT('Ctrl Pts',(90.9474892817076,0.615787752066693,2.00375727084625));
#15250=CARTESIAN_POINT('Ctrl Pts',(91.066639997727,-1.35035406894049,1.60308306366094));
#15251=CARTESIAN_POINT('Ctrl Pts',(91.185790713746,-2.07910482788197,-0.266301222520941));
#15252=CARTESIAN_POINT('Ctrl Pts',(91.3049414297653,-0.902640265067203,
-1.89180332658395));
#15253=CARTESIAN_POINT('Ctrl Pts',(91.4240921457842,1.10096224806914,-1.78366156273085));
#15254=CARTESIAN_POINT('Ctrl Pts',(91.5432428618034,2.09569043340321,-0.0410822156528534));
#15255=CARTESIAN_POINT('Ctrl Pts',(91.6623935778227,1.17001280663651,1.73916158556239));
#15256=CARTESIAN_POINT('Ctrl Pts',(91.7815442938416,-0.827815945467298,
1.92569987629852));
#15257=CARTESIAN_POINT('Ctrl Pts',(91.9006950098609,-2.06706844074748,0.347610502843638));
#15258=CARTESIAN_POINT('Ctrl Pts',(92.0198457258799,-1.41214414015499,-1.54901719283562));
#15259=CARTESIAN_POINT('Ctrl Pts',(92.1389964418991,0.536810999374776,-2.02618796151878));
#15260=CARTESIAN_POINT('Ctrl Pts',(92.2581471579182,1.99385461541733,-0.64664385891275));
#15261=CARTESIAN_POINT('Ctrl Pts',(92.3772978739375,1.62381170543408,1.32545842158787));
#15262=CARTESIAN_POINT('Ctrl Pts',(92.4964485899565,-0.234225573255156,
2.08296487592058));
#15263=CARTESIAN_POINT('Ctrl Pts',(92.6155993059758,-1.87762815784551,0.931727912763529));
#15264=CARTESIAN_POINT('Ctrl Pts',(92.7347500219948,-1.80044938619497,-1.07330629295879));
#15265=CARTESIAN_POINT('Ctrl Pts',(92.853900738014,-0.0734127193897878,
-2.09480665988727));
#15266=CARTESIAN_POINT('Ctrl Pts',(92.9730514540332,1.72089634993666,-1.19671221974878));
#15267=CARTESIAN_POINT('Ctrl Pts',(93.0922021700523,1.93824665886355,0.798000169787126));
#15268=CARTESIAN_POINT('Ctrl Pts',(93.2113528860714,0.379467308499514,2.06145796491198));
#15269=CARTESIAN_POINT('Ctrl Pts',(93.3305036020905,-1.52704030362853,1.43588031962378));
#15270=CARTESIAN_POINT('Ctrl Pts',(93.4496543181096,-2.03423087728717,-0.505479098115718));
#15271=CARTESIAN_POINT('Ctrl Pts',(93.5688050341289,-0.67733579459438,-1.98363822353627));
#15272=CARTESIAN_POINT('Ctrl Pts',(93.6879557501479,1.3002420008455,-1.64407272344841));
#15273=CARTESIAN_POINT('Ctrl Pts',(93.8071064661672,2.08633141084316,0.202053519661223));
#15274=CARTESIAN_POINT('Ctrl Pts',(93.9262571821861,0.960592374618062,1.86302621304239));
#15275=CARTESIAN_POINT('Ctrl Pts',(94.0454078982054,-1.04539407459211,1.81679817522325));
#15276=CARTESIAN_POINT('Ctrl Pts',(94.1645586142245,-2.0934243146716,0.10573088204438));
#15277=CARTESIAN_POINT('Ctrl Pts',(94.2837093302435,-1.22312646267178,-1.70222385043407));
#15278=CARTESIAN_POINT('Ctrl Pts',(94.4028600462628,0.767994261721968,-1.95033053471462));
#15279=CARTESIAN_POINT('Ctrl Pts',(94.5220107622818,2.05535657627397,-0.411234391854458));
#15280=CARTESIAN_POINT('Ctrl Pts',(94.6411614783011,1.45927451126389,1.504700063618));
#15281=CARTESIAN_POINT('Ctrl Pts',(94.7603121943202,-0.474026802320936,
2.04178915937917));
#15282=CARTESIAN_POINT('Ctrl Pts',(94.8794629103393,-1.97294941641427,0.707866499381977));
#15283=CARTESIAN_POINT('Ctrl Pts',(94.9986136263584,-1.66394218884373,-1.27471595771868));
#15284=CARTESIAN_POINT('Ctrl Pts',(95.1177643423775,0.169833343978903,-2.08920104727853));
#15285=CARTESIAN_POINT('Ctrl Pts',(95.2369150583968,1.84798057324012,-0.989228073602758));
#15286=CARTESIAN_POINT('Ctrl Pts',(95.3560657744157,1.83271427786672,1.01723289190835));
#15287=CARTESIAN_POINT('Ctrl Pts',(95.475216490435,0.138023864149379,2.09154339988488));
#15288=CARTESIAN_POINT('Ctrl Pts',(95.5943672064542,-1.68314595181788,1.2492494088675));
#15289=CARTESIAN_POINT('Ctrl Pts',(95.7135179224733,-1.96194992259393,-0.737805449905584));
#15290=CARTESIAN_POINT('Ctrl Pts',(95.8326686384925,-0.442903536235988,
-2.04876568652113));
#15291=CARTESIAN_POINT('Ctrl Pts',(95.9518193545115,1.48200146640357,-1.48232116434138));
#15292=CARTESIAN_POINT('Ctrl Pts',(96.0709700705307,2.04886117188075,0.442461613065045));
#15293=CARTESIAN_POINT('Ctrl Pts',(96.1901207865498,0.738228619699466,1.96179073443972));
#15294=CARTESIAN_POINT('Ctrl Pts',(96.3092715025689,-1.24888633006439,1.68341537216896));
#15295=CARTESIAN_POINT('Ctrl Pts',(96.4284222185881,-2.0915731225807,-0.13757272104082));
#15296=CARTESIAN_POINT('Ctrl Pts',(96.5475729346072,-1.01762817944508,-1.83249482102335));
#15297=CARTESIAN_POINT('Ctrl Pts',(96.6667236506264,0.988829446494665,-1.84819390390174));
#15298=CARTESIAN_POINT('Ctrl Pts',(96.7858743666454,2.08916436611398,-0.170283974688326));
#15299=CARTESIAN_POINT('Ctrl Pts',(96.9050250826647,1.27507483561182,1.66366719757177));
#15300=CARTESIAN_POINT('Ctrl Pts',(97.0241757986838,-0.707440923399836,
1.97310205528165));
#15301=CARTESIAN_POINT('Ctrl Pts',(97.1433265147031,-2.0416868656614,0.474467199355257));
#15302=CARTESIAN_POINT('Ctrl Pts',(97.262477230722,-1.50501478993517,-1.45894991786086));
#15303=CARTESIAN_POINT('Ctrl Pts',(97.3816279467414,0.410791047792594,-2.05544523049543));
#15304=CARTESIAN_POINT('Ctrl Pts',(97.5007786627603,1.95016483517421,-0.768414924627563));
#15305=CARTESIAN_POINT('Ctrl Pts',(97.6199293787795,1.70248763572999,1.22275926959289));
#15306=CARTESIAN_POINT('Ctrl Pts',(97.7390800947986,-0.105279334044914,
2.09344707149284));
#15307=CARTESIAN_POINT('Ctrl Pts',(97.8582308108178,-1.81657264433298,1.04578592906823));
#15308=CARTESIAN_POINT('Ctrl Pts',(97.9773815268368,-1.86323336697702,-0.960190504173446));
#15309=CARTESIAN_POINT('Ctrl Pts',(98.0965322428562,-0.20250353012914,-2.08628777735995));
#15310=CARTESIAN_POINT('Ctrl Pts',(98.215682958875,1.64379222570971,-1.30059659750868));
#15311=CARTESIAN_POINT('Ctrl Pts',(98.3348336748945,1.98378427883073,0.676907924034713));
#15312=CARTESIAN_POINT('Ctrl Pts',(98.4539843909134,0.505917860014153,2.03412177914799));
#15313=CARTESIAN_POINT('Ctrl Pts',(98.5731351069327,-1.43555089986518,1.52735002404793));
#15314=CARTESIAN_POINT('Ctrl Pts',(98.6922858229516,-2.06153978320217,-0.379022730143428));
#15315=CARTESIAN_POINT('Ctrl Pts',(98.8114365389709,-0.798418193117015,
-1.93807432606522));
#15316=CARTESIAN_POINT('Ctrl Pts',(98.9305872549901,1.19634093511385,-1.72115475865633));
#15317=CARTESIAN_POINT('Ctrl Pts',(99.0497379710091,2.09482257432651,0.0729615139196275));
#15318=CARTESIAN_POINT('Ctrl Pts',(99.1688886870284,1.07369436431878,1.80021656063267));
#15319=CARTESIAN_POINT('Ctrl Pts',(99.2880394030473,-0.931322383403096,
1.87783162359188));
#15320=CARTESIAN_POINT('Ctrl Pts',(99.4071901190665,-2.08291531875349,0.234669802068244));
#15321=CARTESIAN_POINT('Ctrl Pts',(99.5263408350856,-1.32580662471439,-1.62351570238799));
#15322=CARTESIAN_POINT('Ctrl Pts',(99.6454915511049,0.646209757148569,-1.99401409833549));
#15323=CARTESIAN_POINT('Ctrl Pts',(99.764642267124,2.02608012778821,-0.537208099548037));
#15324=CARTESIAN_POINT('Ctrl Pts',(99.8837929831432,1.54930581582797,1.41173046632221));
#15325=CARTESIAN_POINT('Ctrl Pts',(100.002943699162,-0.347132893284113,
2.06730174635073));
#15326=CARTESIAN_POINT('Ctrl Pts',(100.122094415182,-1.92558452479489,0.827915832565954));
#15327=CARTESIAN_POINT('Ctrl Pts',(100.241245131201,-1.73928746259611,-1.1690087168201));
#15328=CARTESIAN_POINT('Ctrl Pts',(100.36039584722,0.0403720537186134,-2.09696051023103));
#15329=CARTESIAN_POINT('Ctrl Pts',(100.479546563239,1.78401058767028,-1.09872853364812));
#15330=CARTESIAN_POINT('Ctrl Pts',(100.558980373919,1.85429484974891,0.230679105954203));
#15331=CARTESIAN_POINT('Ctrl Pts',(100.598697279258,1.60036387061328,0.76317068615848));
#15332=CARTESIAN_POINT('Ctrl Pts',(100.349869898682,-0.0938337030309702,
-1.77668351508385));
#15333=CARTESIAN_POINT('Ctrl Pts',(100.349869898683,-0.0511432819576765,
-1.78421672036904));
#15334=CARTESIAN_POINT('Ctrl Pts',(100.349869898683,-0.00826292637260691,
-1.79006544278202));
#15335=CARTESIAN_POINT('Ctrl Pts',(100.349869898683,0.0347219594181995,
-1.79419129823277));
#15336=CARTESIAN_POINT('Ctrl Pts',(100.349869898683,0.0995747997289633,
-1.80041612446577));
#15337=CARTESIAN_POINT('Ctrl Pts',(100.349869898683,0.164664857862779,-1.80272216545716));
#15338=CARTESIAN_POINT('Ctrl Pts',(100.349869898683,0.229725300885462,-1.80133298954642));
#15339=CARTESIAN_POINT('Ctrl Pts',(100.349869898683,0.29658102383718,-1.79990548067153));
#15340=CARTESIAN_POINT('Ctrl Pts',(100.349869898682,0.363406212846255,-1.79457604187652));
#15341=CARTESIAN_POINT('Ctrl Pts',(100.349869898682,0.429927457817016,-1.78553511431863));
#15342=CARTESIAN_POINT('Ctrl Pts',(100.349869898682,0.461888589270306,-1.78119126485725));
#15343=CARTESIAN_POINT('Ctrl Pts',(100.349869898682,0.493779720820322,-1.77598986775753));
#15344=CARTESIAN_POINT('Ctrl Pts',(100.349869898682,0.525570989728989,-1.76994792489328));
#15345=CARTESIAN_POINT('Ctrl Pts',(100.349869898682,0.54423944949515,-1.76639997694585));
#15346=CARTESIAN_POINT('Ctrl Pts',(100.349869898682,0.562873475889208,-1.76256213670072));
#15347=CARTESIAN_POINT('Ctrl Pts',(100.349869898682,0.581467005198565,-1.75843743329546));
#15348=CARTESIAN_POINT('Ctrl Pts',(100.349869898682,0.596154585183359,-1.75517920780366));
#15349=CARTESIAN_POINT('Ctrl Pts',(100.349869898682,0.61082035890722,-1.75174098890012));
#15350=CARTESIAN_POINT('Ctrl Pts',(100.349869898682,0.62543517443403,-1.74813099328806));
#15351=CARTESIAN_POINT('Ctrl Pts',(100.349869898682,0.693180732655042,-1.73139720917252));
#15352=CARTESIAN_POINT('Ctrl Pts',(100.349869898682,0.75993966088107,-1.71095435092334));
#15353=CARTESIAN_POINT('Ctrl Pts',(100.349869898682,0.825417690190425,-1.68703869995642));
#15354=CARTESIAN_POINT('Ctrl Pts',(100.349869898682,0.893547624512638,-1.66215444875285));
#15355=CARTESIAN_POINT('Ctrl Pts',(100.349869898682,0.960291802375473,-1.63351046803854));
#15356=CARTESIAN_POINT('Ctrl Pts',(100.349869898682,1.02532499042762,-1.60131499980194));
#15357=CARTESIAN_POINT('Ctrl Pts',(100.349869898682,1.09035817847978,-1.56911953156533));
#15358=CARTESIAN_POINT('Ctrl Pts',(100.349869898682,1.15368151098642,-1.5333722334378));
#15359=CARTESIAN_POINT('Ctrl Pts',(100.349869898682,1.21495958037596,-1.49422728705875));
#15360=CARTESIAN_POINT('Ctrl Pts',(100.349869898682,1.23197877907323,-1.48335527971492));
#15361=CARTESIAN_POINT('Ctrl Pts',(100.349869898682,1.24884009337816,-1.47222088111476));
#15362=CARTESIAN_POINT('Ctrl Pts',(100.349869898682,1.26553601308461,-1.46082671008785));
#15363=CARTESIAN_POINT('Ctrl Pts',(100.349869898682,1.27472938384657,-1.45455267184274));
#15364=CARTESIAN_POINT('Ctrl Pts',(100.349869898682,1.28386964618837,-1.44820182666909));
#15365=CARTESIAN_POINT('Ctrl Pts',(100.349869898682,1.29294880238568,-1.44177972141025));
#15366=CARTESIAN_POINT('Ctrl Pts',(100.349869898682,1.35324423929895,-1.39912998237398));
#15367=CARTESIAN_POINT('Ctrl Pts',(100.349869898682,1.4109355605661,-1.35328021420338));
#15368=CARTESIAN_POINT('Ctrl Pts',(100.349869898682,1.46570284855611,-1.30444825220194));
#15369=CARTESIAN_POINT('Ctrl Pts',(100.349869898682,1.52027452518399,-1.25579070246288));
#15370=CARTESIAN_POINT('Ctrl Pts',(100.349869898682,1.57194408034395,-1.20417182322692));
#15371=CARTESIAN_POINT('Ctrl Pts',(100.349869898682,1.6203801336666,-1.14975844255616));
#15372=CARTESIAN_POINT('Ctrl Pts',(100.349869898682,1.6488575513763,-1.11776672432027));
#15373=CARTESIAN_POINT('Ctrl Pts',(100.349869898682,1.67621688115302,-1.08480813782164));
#15374=CARTESIAN_POINT('Ctrl Pts',(100.349869898682,1.7023860920606,-1.05090953536258));
#15375=CARTESIAN_POINT('Ctrl Pts',(100.349869898682,1.73605338905413,-1.00729819680577));
#15376=CARTESIAN_POINT('Ctrl Pts',(100.349869898682,1.76775143347122,-0.96213131021098));
#15377=CARTESIAN_POINT('Ctrl Pts',(100.349869898682,1.79747650045067,-0.91554685912618));
#15378=CARTESIAN_POINT('Ctrl Pts',(100.349869898682,1.80400780711786,-0.905311143386069));
#15379=CARTESIAN_POINT('Ctrl Pts',(100.349869898682,1.81043884326635,-0.895014695114847));
#15380=CARTESIAN_POINT('Ctrl Pts',(100.349869898682,1.81676859411639,-0.884661460495994));
#15381=CARTESIAN_POINT('Ctrl Pts',(100.349869898682,1.85453363415377,-0.822891206158915));
#15382=CARTESIAN_POINT('Ctrl Pts',(100.349869898682,1.88871158707573,-0.759078616801623));
#15383=CARTESIAN_POINT('Ctrl Pts',(100.349869898682,1.91935392695043,-0.693587452891148));
#15384=CARTESIAN_POINT('Ctrl Pts',(100.349869898682,1.95064136899357,-0.626717527044545));
#15385=CARTESIAN_POINT('Ctrl Pts',(100.349869898682,1.97824312877486,-0.558096935083375));
#15386=CARTESIAN_POINT('Ctrl Pts',(100.349869898682,2.00217647139197,-0.488072928118889));
#15387=CARTESIAN_POINT('Ctrl Pts',(100.349869898682,2.02656984762121,-0.416702958019421));
#15388=CARTESIAN_POINT('Ctrl Pts',(100.349869898682,2.04715283797167,-0.343874285935347));
#15389=CARTESIAN_POINT('Ctrl Pts',(100.349869898682,2.0638992034507,-0.269924895638561));
#15390=CARTESIAN_POINT('Ctrl Pts',(100.349869898682,2.06724025486549,-0.255171323265874));
#15391=CARTESIAN_POINT('Ctrl Pts',(100.349869898682,2.07042844291392,-0.240373072421388));
#15392=CARTESIAN_POINT('Ctrl Pts',(100.349869898682,2.07346332983987,-0.22553273542015));
#15393=CARTESIAN_POINT('Ctrl Pts',(100.349869898682,2.07629732325714,-0.211674750461271));
#15394=CARTESIAN_POINT('Ctrl Pts',(100.349869898682,2.07899763861465,-0.197780066263574));
#15395=CARTESIAN_POINT('Ctrl Pts',(100.349869898682,2.08156385697012,-0.183850777550955));
#15396=CARTESIAN_POINT('Ctrl Pts',(100.349869898682,2.08418234040323,-0.169637796940341));
#15397=CARTESIAN_POINT('Ctrl Pts',(100.349869898682,2.08665986231497,-0.155395799266646));
#15398=CARTESIAN_POINT('Ctrl Pts',(100.349869898682,2.08899516018094,-0.141135229261458));
#15399=CARTESIAN_POINT('Ctrl Pts',(100.349869898682,2.10153910007024,-0.064535265060426));
#15400=CARTESIAN_POINT('Ctrl Pts',(100.349869898682,2.1099963385427,0.0126694023299449));
#15401=CARTESIAN_POINT('Ctrl Pts',(100.349869898682,2.11437309453932,0.0901070091513077));
#15402=CARTESIAN_POINT('Ctrl Pts',(100.349869898682,2.11878252606939,0.168122741669996));
#15403=CARTESIAN_POINT('Ctrl Pts',(100.349869898682,2.11905064378886,0.246375886230533));
#15404=CARTESIAN_POINT('Ctrl Pts',(100.349869898682,2.115135354418,0.324505766001785));
#15405=CARTESIAN_POINT('Ctrl Pts',(100.349869898682,2.11414398385949,0.344288636489207));
#15406=CARTESIAN_POINT('Ctrl Pts',(100.349869898682,2.11288414907923,0.364063658710017));
#15407=CARTESIAN_POINT('Ctrl Pts',(100.349869898682,2.11135463994526,0.383825055241076));
#15408=CARTESIAN_POINT('Ctrl Pts',(100.349869898682,2.11020352169231,0.398697607320423));
#15409=CARTESIAN_POINT('Ctrl Pts',(100.349869898682,2.108900401199,0.413552658108748));
#15410=CARTESIAN_POINT('Ctrl Pts',(100.349869898682,2.1074453999023,0.428386817866731));
#15411=CARTESIAN_POINT('Ctrl Pts',(100.349869898682,2.09968291124947,0.507527638604876));
#15412=CARTESIAN_POINT('Ctrl Pts',(100.349869898682,2.08760086542093,0.586080887213785));
#15413=CARTESIAN_POINT('Ctrl Pts',(100.349869898682,2.07117840523179,0.66367273374298));
#15414=CARTESIAN_POINT('Ctrl Pts',(100.349869898682,2.05490267436583,0.740571322441432));
#15415=CARTESIAN_POINT('Ctrl Pts',(100.349869898682,2.03436391310446,0.816526640041535));
#15416=CARTESIAN_POINT('Ctrl Pts',(100.349869898682,2.0094914935604,0.891179159993237));
#15417=CARTESIAN_POINT('Ctrl Pts',(100.349869898682,2.0030758752601,0.910435110236341));
#15418=CARTESIAN_POINT('Ctrl Pts',(100.349869898682,1.99637165302178,0.929604358635609));
#15419=CARTESIAN_POINT('Ctrl Pts',(100.349869898682,1.98937704260618,0.948680653513806));
#15420=CARTESIAN_POINT('Origin',(100.349869898682,0.,0.));
#15421=CARTESIAN_POINT('Origin',(33.1926516271063,0.,0.));
#15422=CARTESIAN_POINT('',(33.4926516271063,-5.13007994755883E-16,4.18902817623056));
#15423=CARTESIAN_POINT('Origin',(33.4926516271063,0.,0.));
#15424=CARTESIAN_POINT('',(33.1926516271063,-5.49747398730303E-16,4.48902817623056));
#15425=CARTESIAN_POINT('Origin',(33.1926516271063,-5.13007994755883E-16,
4.18902817623056));
#15426=CARTESIAN_POINT('Origin',(33.1926516271063,0.,0.));
#15427=CARTESIAN_POINT('Origin',(32.5726008112287,0.,0.));
#15428=CARTESIAN_POINT('',(31.6525499953511,-5.49747398730303E-16,4.48902817623056));
#15429=CARTESIAN_POINT('',(32.5726008112287,-5.49747398730304E-16,4.48902817623056));
#15430=CARTESIAN_POINT('Origin',(31.6525499953511,0.,0.));
#15431=CARTESIAN_POINT('Origin',(33.4926516271063,0.,-2.21164758166987));
#15432=CARTESIAN_POINT('Origin',(31.3525499953512,0.,0.));
#15433=CARTESIAN_POINT('',(31.6525499953511,-7.4821050118432E-16,6.1096023907077));
#15434=CARTESIAN_POINT('Origin',(31.6525499953511,0.,0.));
#15435=CARTESIAN_POINT('',(31.3524613125654,-7.84949903553507E-16,6.40960237759997));
#15436=CARTESIAN_POINT('Origin',(31.3525499953512,-7.4821050118432E-16,
6.1096023907077));
#15437=CARTESIAN_POINT('Origin',(31.3524613125654,-7.84949903553507E-16,
0.));
#15438=CARTESIAN_POINT('Origin',(31.0318089645314,0.,0.));
#15439=CARTESIAN_POINT('',(30.7109792509259,-7.84926680813535E-16,6.40941274953751));
#15440=CARTESIAN_POINT('',(31.0318089645314,-7.84938295393988E-16,6.40950758978419));
#15441=CARTESIAN_POINT('Origin',(30.7109792509259,-7.84926680813535E-16,
0.));
#15442=CARTESIAN_POINT('Origin',(31.6525499953511,0.,-4.48902817623056));
#15443=CARTESIAN_POINT('Origin',(30.7110679337117,0.,0.));
#15444=CARTESIAN_POINT('',(30.4110679337117,-7.48187278444348E-16,6.10941276264524));
#15445=CARTESIAN_POINT('Origin',(30.7110679337117,-7.48187278444348E-16,
6.10941276264524));
#15446=CARTESIAN_POINT('Origin',(30.4110679337117,0.,0.));
#15447=CARTESIAN_POINT('Origin',(30.4110679337117,0.,-6.40932409296331));
#15448=CARTESIAN_POINT('',(30.4110679337117,-2.70848713173399E-16,2.21164758166987));
#15449=CARTESIAN_POINT('Origin',(30.4110679337117,0.,0.));
#15450=CARTESIAN_POINT('Origin',(28.3729800631879,0.,0.));
#15451=CARTESIAN_POINT('',(28.6729800631879,-7.48102635692981E-16,6.1087216021292));
#15452=CARTESIAN_POINT('Origin',(28.6729800631879,0.,0.));
#15453=CARTESIAN_POINT('',(28.3728913804021,-7.84842038062168E-16,6.40872158902147));
#15454=CARTESIAN_POINT('Origin',(28.3729800631879,-7.48102635692982E-16,
6.1087216021292));
#15455=CARTESIAN_POINT('Origin',(28.3728913804021,-7.84842038062168E-16,
0.));
#15456=CARTESIAN_POINT('Origin',(28.2136282688352,0.,0.));
#15457=CARTESIAN_POINT('',(28.0541877916966,-7.84830500451046E-16,6.40862737727707));
#15458=CARTESIAN_POINT('',(28.2136282688352,-7.84836272467075E-16,6.40867450936473));
#15459=CARTESIAN_POINT('Origin',(28.0541877916966,-7.84830500451046E-16,
0.));
#15460=CARTESIAN_POINT('Origin',(28.6729800631879,0.,0.));
#15461=CARTESIAN_POINT('',(28.6729800631879,-2.70848713173399E-16,2.21164758166987));
#15462=CARTESIAN_POINT('Origin',(28.6729800631879,0.,0.));
#15463=CARTESIAN_POINT('Origin',(28.0542764744824,0.,0.));
#15464=CARTESIAN_POINT('Origin',(28.0542764744824,-7.4809109808186E-16,
6.1086273903848));
#15465=CARTESIAN_POINT('Origin',(25.1947388265965,0.,0.));
#15466=CARTESIAN_POINT('',(25.1946501438108,-7.84726980332233E-16,6.40778207135796));
#15467=CARTESIAN_POINT('Origin',(25.1947388265965,-7.47987577963046E-16,
6.10778208446569));
#15468=CARTESIAN_POINT('Origin',(25.1946501438108,-7.84726980332233E-16,
0.));
#15469=CARTESIAN_POINT('Origin',(25.0105689136245,0.,0.));
#15470=CARTESIAN_POINT('',(24.8263103178667,-7.84713645805033E-16,6.40767318668028));
#15471=CARTESIAN_POINT('',(25.0105689136245,-7.847203162791E-16,6.40772765523458));
#15472=CARTESIAN_POINT('Origin',(24.8263103178667,-7.84713645805033E-16,
0.));
#15473=CARTESIAN_POINT('Origin',(24.8263990006525,0.,0.));
#15474=CARTESIAN_POINT('',(24.5263990006525,-7.47974243435846E-16,6.10767319978801));
#15475=CARTESIAN_POINT('Origin',(24.8263990006525,-7.47974243435846E-16,
6.10767319978801));
#15476=CARTESIAN_POINT('Origin',(24.5263990006525,0.,0.));
#15477=CARTESIAN_POINT('Origin',(24.5263990006525,0.,-6.40758453010608));
#15478=CARTESIAN_POINT('',(24.5263990006525,-2.70848713173399E-16,2.21164758166987));
#15479=CARTESIAN_POINT('Origin',(24.5263990006525,0.,0.));
#15480=CARTESIAN_POINT('Origin',(22.4730782633311,0.,0.));
#15481=CARTESIAN_POINT('',(22.7730782633312,-7.47889049228833E-16,6.1069775362949));
#15482=CARTESIAN_POINT('Origin',(22.7730782633312,0.,0.));
#15483=CARTESIAN_POINT('',(22.4729895805454,-7.8462845159802E-16,6.40697752318717));
#15484=CARTESIAN_POINT('Origin',(22.4730782633311,-7.47889049228834E-16,
6.1069775362949));
#15485=CARTESIAN_POINT('Origin',(22.4729895805454,-7.8462845159802E-16,
0.));
#15486=CARTESIAN_POINT('Origin',(22.2310089528171,0.,0.));
#15487=CARTESIAN_POINT('',(21.9888509595172,-7.84610924957793E-16,6.40683440730886));
#15488=CARTESIAN_POINT('',(22.2310089528171,-7.84619691488374E-16,6.40690599146347));
#15489=CARTESIAN_POINT('Origin',(21.9888509595172,-7.84610924957793E-16,
0.));
#15490=CARTESIAN_POINT('Origin',(22.7730782633312,0.,-2.21164758166987));
#15491=CARTESIAN_POINT('',(22.7730782633312,-2.70848713173399E-16,2.21164758166987));
#15492=CARTESIAN_POINT('Origin',(22.7730782633312,0.,0.));
#15493=CARTESIAN_POINT('Origin',(21.9889396423029,0.,0.));
#15494=CARTESIAN_POINT('',(21.688939642303,-7.47871522588606E-16,6.10683442041659));
#15495=CARTESIAN_POINT('Origin',(21.9889396423029,-7.47871522588606E-16,
6.10683442041659));
#15496=CARTESIAN_POINT('Origin',(21.688939642303,0.,0.));
#15497=CARTESIAN_POINT('Origin',(21.688939642303,0.,-6.40674575073467));
#15498=CARTESIAN_POINT('',(21.688939642303,-5.41697426346798E-16,4.42329516333974));
#15499=CARTESIAN_POINT('Origin',(21.688939642303,0.,0.));
#15500=CARTESIAN_POINT('Origin',(21.1989257366328,0.,0.));
#15501=CARTESIAN_POINT('',(21.1989257366328,-5.41697426346798E-16,4.42329516333974));
#15502=CARTESIAN_POINT('Origin',(21.1989257366328,0.,0.));
#15503=CARTESIAN_POINT('',(20.8989257366328,-5.04958022372377E-16,4.12329516333974));
#15504=CARTESIAN_POINT('Origin',(21.1989257366328,-5.04958022372377E-16,
4.12329516333974));
#15505=CARTESIAN_POINT('Origin',(20.8989257366328,0.,0.));
#15506=CARTESIAN_POINT('Origin',(20.8989257366328,0.,-4.42329516333974));
#15507=CARTESIAN_POINT('Origin',(21.2939326894679,0.,0.));
#15508=CARTESIAN_POINT('',(21.2939326894679,-5.41697426346798E-16,4.42329516333974));
#15509=CARTESIAN_POINT('Origin',(23.6497386319918,0.,0.));
#15510=CARTESIAN_POINT('',(23.6497386319918,-2.70848713173399E-16,2.21164758166987));
#15511=CARTESIAN_POINT('Origin',(29.5420239984498,0.,0.));
#15512=CARTESIAN_POINT('',(29.5420239984498,-2.70848713173399E-16,2.21164758166987));
#15513=CARTESIAN_POINT('',(0.,0.,0.));
#15514=CARTESIAN_POINT('Ctrl Pts',(6.4430005297901,1.97158113240038,3.97043534620107));
#15515=CARTESIAN_POINT('Ctrl Pts',(11.2430005297901,1.97158113240038,3.97043534620107));
#15516=CARTESIAN_POINT('Ctrl Pts',(6.4430005297901,2.29671111436096,3.77621792657107));
#15517=CARTESIAN_POINT('Ctrl Pts',(11.2430005297901,2.29671111436096,3.77621792657107));
#15518=CARTESIAN_POINT('Ctrl Pts',(6.4430005297901,2.59552275281558,3.54102114079632));
#15519=CARTESIAN_POINT('Ctrl Pts',(11.2430005297901,2.59552275281558,3.54102114079632));
#15520=CARTESIAN_POINT('Ctrl Pts',(6.4430005297901,3.11908576775695,3.00435277140383));
#15521=CARTESIAN_POINT('Ctrl Pts',(11.2430005297901,3.11908576775695,3.00435277140383));
#15522=CARTESIAN_POINT('Ctrl Pts',(6.4430005297901,3.34301024132503,2.70651491388494));
#15523=CARTESIAN_POINT('Ctrl Pts',(11.2430005297901,3.34301024132503,2.70651491388494));
#15524=CARTESIAN_POINT('Ctrl Pts',(6.4430005297901,3.79251211736076,1.90981794028965));
#15525=CARTESIAN_POINT('Ctrl Pts',(11.2430005297901,3.79251211736076,1.90981794028965));
#15526=CARTESIAN_POINT('Ctrl Pts',(6.4430005297901,3.96610878107774,1.3893796287376));
#15527=CARTESIAN_POINT('Ctrl Pts',(11.2430005297901,3.96610878107774,1.3893796287376));
#15528=CARTESIAN_POINT('Ctrl Pts',(6.4430005297901,4.09877879619631,0.327978495265378));
#15529=CARTESIAN_POINT('Ctrl Pts',(11.2430005297901,4.09877879619631,0.327978495265378));
#15530=CARTESIAN_POINT('Ctrl Pts',(6.4430005297901,4.06307606785725,-0.201870082003989));
#15531=CARTESIAN_POINT('Ctrl Pts',(11.2430005297901,4.06307606785725,-0.201870082003989));
#15532=CARTESIAN_POINT('Ctrl Pts',(6.4430005297901,3.79206680758235,-1.20058842967181));
#15533=CARTESIAN_POINT('Ctrl Pts',(11.2430005297901,3.79206680758235,-1.20058842967181));
#15534=CARTESIAN_POINT('Ctrl Pts',(6.4430005297901,3.56572122172907,-1.66148594501202));
#15535=CARTESIAN_POINT('Ctrl Pts',(11.2430005297901,3.56572122172907,-1.66148594501202));
#15536=CARTESIAN_POINT('Ctrl Pts',(6.4430005297901,2.95711124459234,-2.45497912282895));
#15537=CARTESIAN_POINT('Ctrl Pts',(11.2430005297901,2.95711124459234,-2.45497912282895));
#15538=CARTESIAN_POINT('Ctrl Pts',(6.4430005297901,2.58595465431403,-2.78386901588454));
#15539=CARTESIAN_POINT('Ctrl Pts',(11.2430005297901,2.58595465431403,-2.78386901588454));
#15540=CARTESIAN_POINT('Ctrl Pts',(6.4430005297901,2.16151778945146,-3.03095833168072));
#15541=CARTESIAN_POINT('Ctrl Pts',(11.2430005297901,2.16151778945146,-3.03095833168072));
#15542=CARTESIAN_POINT('',(6.4430005297901,1.97158113240038,3.97043534620107));
#15543=CARTESIAN_POINT('',(6.4430005297901,2.16151778945147,-3.03095833168073));
#15544=CARTESIAN_POINT('Ctrl Pts',(6.4430005297901,1.97158113240038,3.97043534620107));
#15545=CARTESIAN_POINT('Ctrl Pts',(6.4430005297901,2.29671111436096,3.77621792657107));
#15546=CARTESIAN_POINT('Ctrl Pts',(6.4430005297901,2.59552275281558,3.54102114079632));
#15547=CARTESIAN_POINT('Ctrl Pts',(6.4430005297901,3.11908576775695,3.00435277140383));
#15548=CARTESIAN_POINT('Ctrl Pts',(6.4430005297901,3.34301024132503,2.70651491388494));
#15549=CARTESIAN_POINT('Ctrl Pts',(6.4430005297901,3.79251211736076,1.90981794028965));
#15550=CARTESIAN_POINT('Ctrl Pts',(6.4430005297901,3.96610878107774,1.3893796287376));
#15551=CARTESIAN_POINT('Ctrl Pts',(6.4430005297901,4.09877879619631,0.327978495265378));
#15552=CARTESIAN_POINT('Ctrl Pts',(6.4430005297901,4.06307606785725,-0.201870082003989));
#15553=CARTESIAN_POINT('Ctrl Pts',(6.4430005297901,3.79206680758235,-1.20058842967181));
#15554=CARTESIAN_POINT('Ctrl Pts',(6.4430005297901,3.56572122172907,-1.66148594501202));
#15555=CARTESIAN_POINT('Ctrl Pts',(6.4430005297901,2.95711124459234,-2.45497912282895));
#15556=CARTESIAN_POINT('Ctrl Pts',(6.4430005297901,2.58595465431403,-2.78386901588454));
#15557=CARTESIAN_POINT('Ctrl Pts',(6.4430005297901,2.16151778945146,-3.03095833168072));
#15558=CARTESIAN_POINT('',(10.4430005297901,2.16151778945147,-3.03095833168073));
#15559=CARTESIAN_POINT('',(6.4430005297901,2.16151778945147,-3.03095833168073));
#15560=CARTESIAN_POINT('',(10.4430005297901,1.97158113240038,3.97043534620107));
#15561=CARTESIAN_POINT('Ctrl Pts',(10.4430005297901,1.97158113240038,3.97043534620107));
#15562=CARTESIAN_POINT('Ctrl Pts',(10.4430005297901,2.29671111436096,3.77621792657107));
#15563=CARTESIAN_POINT('Ctrl Pts',(10.4430005297901,2.59552275281558,3.54102114079632));
#15564=CARTESIAN_POINT('Ctrl Pts',(10.4430005297901,3.11908576775695,3.00435277140383));
#15565=CARTESIAN_POINT('Ctrl Pts',(10.4430005297901,3.34301024132503,2.70651491388494));
#15566=CARTESIAN_POINT('Ctrl Pts',(10.4430005297901,3.79251211736076,1.90981794028965));
#15567=CARTESIAN_POINT('Ctrl Pts',(10.4430005297901,3.96610878107774,1.3893796287376));
#15568=CARTESIAN_POINT('Ctrl Pts',(10.4430005297901,4.09877879619631,0.327978495265378));
#15569=CARTESIAN_POINT('Ctrl Pts',(10.4430005297901,4.06307606785725,-0.201870082003989));
#15570=CARTESIAN_POINT('Ctrl Pts',(10.4430005297901,3.79206680758235,-1.20058842967181));
#15571=CARTESIAN_POINT('Ctrl Pts',(10.4430005297901,3.56572122172907,-1.66148594501202));
#15572=CARTESIAN_POINT('Ctrl Pts',(10.4430005297901,2.95711124459234,-2.45497912282895));
#15573=CARTESIAN_POINT('Ctrl Pts',(10.4430005297901,2.58595465431403,-2.78386901588454));
#15574=CARTESIAN_POINT('Ctrl Pts',(10.4430005297901,2.16151778945146,-3.03095833168072));
#15575=CARTESIAN_POINT('',(6.4430005297901,1.97158113240038,3.97043534620107));
#15576=CARTESIAN_POINT('Origin',(6.4430005297901,-2.77555756156289E-16,
5.55111512312578E-16));
#15577=CARTESIAN_POINT('',(6.4430005297901,-1.97158113240039,3.97043534620107));
#15578=CARTESIAN_POINT('Origin',(6.4430005297901,-2.77555756156289E-16,
5.55111512312578E-16));
#15579=CARTESIAN_POINT('',(10.4430005297901,-1.97158113240039,3.97043534620107));
#15580=CARTESIAN_POINT('Origin',(10.4430005297901,-2.77555756156289E-16,
5.55111512312578E-16));
#15581=CARTESIAN_POINT('',(6.4430005297901,-1.97158113240039,3.97043534620107));
#15582=CARTESIAN_POINT('Ctrl Pts',(6.4430005297901,-2.16151778945139,-3.03095833168078));
#15583=CARTESIAN_POINT('Ctrl Pts',(11.2430005297901,-2.16151778945139,-3.03095833168078));
#15584=CARTESIAN_POINT('Ctrl Pts',(6.4430005297901,-2.4417969811413,-2.86779155838698));
#15585=CARTESIAN_POINT('Ctrl Pts',(11.2430005297901,-2.4417969811413,-2.86779155838698));
#15586=CARTESIAN_POINT('Ctrl Pts',(6.4430005297901,-2.69946597133354,-2.66855779259647));
#15587=CARTESIAN_POINT('Ctrl Pts',(11.2430005297901,-2.69946597133354,-2.66855779259647));
#15588=CARTESIAN_POINT('Ctrl Pts',(6.4430005297901,-3.16313807023027,-2.20413689736136));
#15589=CARTESIAN_POINT('Ctrl Pts',(11.2430005297901,-3.16313807023027,-2.20413689736136));
#15590=CARTESIAN_POINT('Ctrl Pts',(6.4430005297901,-3.36582061002206,-1.93954623621156));
#15591=CARTESIAN_POINT('Ctrl Pts',(11.2430005297901,-3.36582061002206,-1.93954623621156));
#15592=CARTESIAN_POINT('Ctrl Pts',(6.4430005297901,-3.7905877946382,-1.20735040930033));
#15593=CARTESIAN_POINT('Ctrl Pts',(11.2430005297901,-3.7905877946382,-1.20735040930033));
#15594=CARTESIAN_POINT('Ctrl Pts',(6.4430005297901,-3.95787261855977,-0.715467908482556));
#15595=CARTESIAN_POINT('Ctrl Pts',(11.2430005297901,-3.95787261855977,-0.715467908482556));
#15596=CARTESIAN_POINT('Ctrl Pts',(6.4430005297901,-4.0999785741866,0.321696095215354));
#15597=CARTESIAN_POINT('Ctrl Pts',(11.2430005297901,-4.0999785741866,0.321696095215354));
#15598=CARTESIAN_POINT('Ctrl Pts',(6.4430005297901,-4.06691955087291,0.857794436836504));
#15599=CARTESIAN_POINT('Ctrl Pts',(11.2430005297901,-4.06691955087291,0.857794436836504));
#15600=CARTESIAN_POINT('Ctrl Pts',(6.4430005297901,-3.79581350913489,1.90493582172488));
#15601=CARTESIAN_POINT('Ctrl Pts',(11.2430005297901,-3.79581350913489,1.90493582172488));
#15602=CARTESIAN_POINT('Ctrl Pts',(6.4430005297901,-3.55404702294629,2.40416273654669));
#15603=CARTESIAN_POINT('Ctrl Pts',(11.2430005297901,-3.55404702294629,2.40416273654669));
#15604=CARTESIAN_POINT('Ctrl Pts',(6.4430005297901,-2.88474862400959,3.29779955123577));
#15605=CARTESIAN_POINT('Ctrl Pts',(11.2430005297901,-2.88474862400959,3.29779955123577));
#15606=CARTESIAN_POINT('Ctrl Pts',(6.4430005297901,-2.45846445810197,3.67959405679302));
#15607=CARTESIAN_POINT('Ctrl Pts',(11.2430005297901,-2.45846445810197,3.67959405679302));
#15608=CARTESIAN_POINT('Ctrl Pts',(6.4430005297901,-1.9715811324004,3.97043534620107));
#15609=CARTESIAN_POINT('Ctrl Pts',(11.2430005297901,-1.9715811324004,3.97043534620107));
#15610=CARTESIAN_POINT('',(6.4430005297901,-2.16151778945139,-3.03095833168078));
#15611=CARTESIAN_POINT('Ctrl Pts',(6.4430005297901,-2.16151778945139,-3.03095833168078));
#15612=CARTESIAN_POINT('Ctrl Pts',(6.4430005297901,-2.4417969811413,-2.86779155838698));
#15613=CARTESIAN_POINT('Ctrl Pts',(6.4430005297901,-2.69946597133354,-2.66855779259647));
#15614=CARTESIAN_POINT('Ctrl Pts',(6.4430005297901,-3.16313807023027,-2.20413689736136));
#15615=CARTESIAN_POINT('Ctrl Pts',(6.4430005297901,-3.36582061002206,-1.93954623621156));
#15616=CARTESIAN_POINT('Ctrl Pts',(6.4430005297901,-3.7905877946382,-1.20735040930033));
#15617=CARTESIAN_POINT('Ctrl Pts',(6.4430005297901,-3.95787261855977,-0.715467908482556));
#15618=CARTESIAN_POINT('Ctrl Pts',(6.4430005297901,-4.0999785741866,0.321696095215354));
#15619=CARTESIAN_POINT('Ctrl Pts',(6.4430005297901,-4.06691955087291,0.857794436836504));
#15620=CARTESIAN_POINT('Ctrl Pts',(6.4430005297901,-3.79581350913489,1.90493582172488));
#15621=CARTESIAN_POINT('Ctrl Pts',(6.4430005297901,-3.55404702294629,2.40416273654669));
#15622=CARTESIAN_POINT('Ctrl Pts',(6.4430005297901,-2.88474862400959,3.29779955123577));
#15623=CARTESIAN_POINT('Ctrl Pts',(6.4430005297901,-2.45846445810197,3.67959405679302));
#15624=CARTESIAN_POINT('Ctrl Pts',(6.4430005297901,-1.9715811324004,3.97043534620107));
#15625=CARTESIAN_POINT('',(10.4430005297901,-2.16151778945139,-3.03095833168078));
#15626=CARTESIAN_POINT('Ctrl Pts',(10.4430005297901,-2.16151778945139,-3.03095833168078));
#15627=CARTESIAN_POINT('Ctrl Pts',(10.4430005297901,-2.4417969811413,-2.86779155838698));
#15628=CARTESIAN_POINT('Ctrl Pts',(10.4430005297901,-2.69946597133354,-2.66855779259647));
#15629=CARTESIAN_POINT('Ctrl Pts',(10.4430005297901,-3.16313807023027,-2.20413689736136));
#15630=CARTESIAN_POINT('Ctrl Pts',(10.4430005297901,-3.36582061002206,-1.93954623621156));
#15631=CARTESIAN_POINT('Ctrl Pts',(10.4430005297901,-3.7905877946382,-1.20735040930033));
#15632=CARTESIAN_POINT('Ctrl Pts',(10.4430005297901,-3.95787261855977,-0.715467908482556));
#15633=CARTESIAN_POINT('Ctrl Pts',(10.4430005297901,-4.0999785741866,0.321696095215354));
#15634=CARTESIAN_POINT('Ctrl Pts',(10.4430005297901,-4.06691955087291,0.857794436836504));
#15635=CARTESIAN_POINT('Ctrl Pts',(10.4430005297901,-3.79581350913489,1.90493582172488));
#15636=CARTESIAN_POINT('Ctrl Pts',(10.4430005297901,-3.55404702294629,2.40416273654669));
#15637=CARTESIAN_POINT('Ctrl Pts',(10.4430005297901,-2.88474862400959,3.29779955123577));
#15638=CARTESIAN_POINT('Ctrl Pts',(10.4430005297901,-2.45846445810197,3.67959405679302));
#15639=CARTESIAN_POINT('Ctrl Pts',(10.4430005297901,-1.9715811324004,3.97043534620107));
#15640=CARTESIAN_POINT('',(6.4430005297901,-2.16151778945139,-3.03095833168078));
#15641=CARTESIAN_POINT('Origin',(6.4430005297901,-2.77555756156289E-16,
5.55111512312578E-16));
#15642=CARTESIAN_POINT('Origin',(6.4430005297901,-2.77555756156289E-16,
5.55111512312578E-16));
#15643=CARTESIAN_POINT('Origin',(10.4430005297901,-2.77555756156289E-16,
5.55111512312578E-16));
#15644=CARTESIAN_POINT('Origin',(6.4430005297901,7.33246945257534,-3.33066907387547E-15));
#15645=CARTESIAN_POINT('',(6.4430005297901,7.33246945257534,-3.33066907387547E-15));
#15646=CARTESIAN_POINT('',(6.4430005297901,3.66623472628768,6.35010481840362));
#15647=CARTESIAN_POINT('',(6.4430005297901,7.33246945257534,-3.33066907387547E-15));
#15648=CARTESIAN_POINT('',(10.4430005297901,3.66623472628768,6.35010481840362));
#15649=CARTESIAN_POINT('',(6.4430005297901,3.66623472628768,6.35010481840362));
#15650=CARTESIAN_POINT('',(10.4430005297901,7.33246945257534,-3.33066907387547E-15));
#15651=CARTESIAN_POINT('',(10.4430005297901,7.33246945257534,-3.33066907387547E-15));
#15652=CARTESIAN_POINT('',(6.4430005297901,7.33246945257534,-3.33066907387547E-15));
#15653=CARTESIAN_POINT('Origin',(6.4430005297901,3.66623472628767,-6.35010481840363));
#15654=CARTESIAN_POINT('',(6.4430005297901,3.66623472628767,-6.35010481840363));
#15655=CARTESIAN_POINT('',(6.4430005297901,3.66623472628767,-6.35010481840363));
#15656=CARTESIAN_POINT('',(10.4430005297901,3.66623472628767,-6.35010481840363));
#15657=CARTESIAN_POINT('',(10.4430005297901,3.66623472628767,-6.35010481840363));
#15658=CARTESIAN_POINT('',(6.4430005297901,3.66623472628767,-6.35010481840363));
#15659=CARTESIAN_POINT('Origin',(6.4430005297901,-3.66623472628767,-6.35010481840362));
#15660=CARTESIAN_POINT('',(6.4430005297901,-3.66623472628767,-6.35010481840362));
#15661=CARTESIAN_POINT('',(6.4430005297901,-3.66623472628767,-6.35010481840362));
#15662=CARTESIAN_POINT('',(10.4430005297901,-3.66623472628767,-6.35010481840362));
#15663=CARTESIAN_POINT('',(10.4430005297901,-3.66623472628767,-6.35010481840362));
#15664=CARTESIAN_POINT('',(6.4430005297901,-3.66623472628767,-6.35010481840362));
#15665=CARTESIAN_POINT('Origin',(6.4430005297901,-7.33246945257535,2.77555756156289E-15));
#15666=CARTESIAN_POINT('',(6.4430005297901,-7.33246945257535,2.77555756156289E-15));
#15667=CARTESIAN_POINT('',(6.4430005297901,-7.33246945257535,2.77555756156289E-15));
#15668=CARTESIAN_POINT('',(10.4430005297901,-7.33246945257535,2.77555756156289E-15));
#15669=CARTESIAN_POINT('',(10.4430005297901,-7.33246945257535,2.77555756156289E-15));
#15670=CARTESIAN_POINT('',(6.4430005297901,-7.33246945257535,2.77555756156289E-15));
#15671=CARTESIAN_POINT('Origin',(6.4430005297901,-3.66623472628767,6.35010481840363));
#15672=CARTESIAN_POINT('',(6.4430005297901,-3.66623472628767,6.35010481840363));
#15673=CARTESIAN_POINT('',(6.4430005297901,-3.66623472628767,6.35010481840363));
#15674=CARTESIAN_POINT('',(10.4430005297901,-3.66623472628767,6.35010481840363));
#15675=CARTESIAN_POINT('',(10.4430005297901,-3.66623472628767,6.35010481840363));
#15676=CARTESIAN_POINT('',(6.4430005297901,-3.66623472628767,6.35010481840363));
#15677=CARTESIAN_POINT('Origin',(6.4430005297901,3.66623472628768,6.35010481840362));
#15678=CARTESIAN_POINT('',(6.4430005297901,3.66623472628768,6.35010481840362));
#15679=CARTESIAN_POINT('',(10.4430005297901,3.66623472628768,6.35010481840362));
#15680=CARTESIAN_POINT('Origin',(10.4430005297901,0.,0.));
#15681=CARTESIAN_POINT('Origin',(6.4430005297901,0.,0.));
#15682=CARTESIAN_POINT('',(0.,0.,0.));
#15683=CARTESIAN_POINT('Origin',(80.1322559480305,0.,0.));
#15684=CARTESIAN_POINT('',(83.3465449346096,-2.62112000711956,2.64359555733806));
#15685=CARTESIAN_POINT('',(83.100211836361,-2.62112000711957,2.64359555733806));
#15686=CARTESIAN_POINT('',(80.1322559480305,-2.62112000711956,2.64359555733806));
#15687=CARTESIAN_POINT('',(82.4430056483001,-2.16413257099361,-3.02909190644071));
#15688=CARTESIAN_POINT('Ctrl Pts',(82.4430056483001,-2.16413257099361,-3.02909190644071));
#15689=CARTESIAN_POINT('Ctrl Pts',(82.4488434649895,-2.07571222369529,-3.09226376105495));
#15690=CARTESIAN_POINT('Ctrl Pts',(82.4546812816788,-1.98435154649692,-3.15168333584861));
#15691=CARTESIAN_POINT('Ctrl Pts',(82.4605190983682,-1.89040984780533,-3.20705755636232));
#15692=CARTESIAN_POINT('Ctrl Pts',(82.4663495706933,-1.79658633406051,-3.26236211239906));
#15693=CARTESIAN_POINT('Ctrl Pts',(82.4721800430184,-1.70018862181831,-3.31363120595717));
#15694=CARTESIAN_POINT('Ctrl Pts',(82.4780105153435,-1.60160744862291,-3.36061320937349));
#15695=CARTESIAN_POINT('Ctrl Pts',(82.4839136640581,-1.50179746867793,-3.40818083985263));
#15696=CARTESIAN_POINT('Ctrl Pts',(82.4898168127728,-1.39974957584534,-3.45135348923295));
#15697=CARTESIAN_POINT('Ctrl Pts',(82.4957199614874,-1.29589809170575,-3.48991628816701));
#15698=CARTESIAN_POINT('Ctrl Pts',(82.501541268857,-1.19348640614775,-3.5279444518605));
#15699=CARTESIAN_POINT('Ctrl Pts',(82.5073625762267,-1.08932124388746,-3.56148961867586));
#15700=CARTESIAN_POINT('Ctrl Pts',(82.5131838835963,-0.983840973759557,
-3.590393362969));
#15701=CARTESIAN_POINT('Ctrl Pts',(82.5190035462291,-0.878390505748904,
-3.61928894087448));
#15702=CARTESIAN_POINT('Ctrl Pts',(82.5248232088619,-0.771626088111857,
-3.64354558595605));
#15703=CARTESIAN_POINT('Ctrl Pts',(82.5306428714946,-0.664001330539854,
-3.66305470823755));
#15704=CARTESIAN_POINT('Ctrl Pts',(82.5364624586586,-0.556377968634886,
-3.68256357752672));
#15705=CARTESIAN_POINT('Ctrl Pts',(82.5422820458226,-0.447894718211021,
-3.69732496970828));
#15706=CARTESIAN_POINT('Ctrl Pts',(82.5481016329866,-0.339014446828578,
-3.70728158727409));
#15707=CARTESIAN_POINT('Ctrl Pts',(82.5540670039457,-0.22740666596446,-3.71748762347628));
#15708=CARTESIAN_POINT('Ctrl Pts',(82.5600323749047,-0.11538218645221,-3.72264489477563));
#15709=CARTESIAN_POINT('Ctrl Pts',(82.5659977458638,-0.00344252263953471,
-3.72274840830506));
#15710=CARTESIAN_POINT('Ctrl Pts',(82.5718250423947,0.105906186617274,-3.72284952591118));
#15711=CARTESIAN_POINT('Ctrl Pts',(82.5776523389257,0.215173525287183,-3.71812837826768));
#15712=CARTESIAN_POINT('Ctrl Pts',(82.5834796354566,0.323895920577596,-3.70863303592216));
#15713=CARTESIAN_POINT('Ctrl Pts',(82.5895140436297,0.436482487479869,-3.69880021359159));
#15714=CARTESIAN_POINT('Ctrl Pts',(82.5955484518028,0.548484139555762,-3.6838475851159));
#15715=CARTESIAN_POINT('Ctrl Pts',(82.6015828599759,0.659397897522503,-3.66388618481018));
#15716=CARTESIAN_POINT('Ctrl Pts',(82.607617268149,0.770311655489244,-3.64392478450446));
#15717=CARTESIAN_POINT('Ctrl Pts',(82.6136516763221,0.880137038913179,-3.61895480083851));
#15718=CARTESIAN_POINT('Ctrl Pts',(82.6196860844952,0.988390395894478,-3.58914362875095));
#15719=CARTESIAN_POINT('Ctrl Pts',(82.6256670228396,1.09568453893299,-3.55959660821227));
#15720=CARTESIAN_POINT('Ctrl Pts',(82.631647961184,1.20181842618435,-3.52518858032981));
#15721=CARTESIAN_POINT('Ctrl Pts',(82.6376288995284,1.30632173434007,-3.48602798165631));
#15722=CARTESIAN_POINT('Ctrl Pts',(82.6436023926444,1.41069495404613,-3.44691613111967));
#15723=CARTESIAN_POINT('Ctrl Pts',(82.6495758857604,1.51344124667461,-3.40306362073061));
#15724=CARTESIAN_POINT('Ctrl Pts',(82.6555493788764,1.61410380075984,-3.3546291125656));
#15725=CARTESIAN_POINT('Ctrl Pts',(82.6615170319686,1.71466794145509,-3.30624195670734));
#15726=CARTESIAN_POINT('Ctrl Pts',(82.6674846850609,1.81315202466722,-3.25328189334218));
#15727=CARTESIAN_POINT('Ctrl Pts',(82.6734523381531,1.90911829154975,-3.19595602463022));
#15728=CARTESIAN_POINT('Ctrl Pts',(82.679415920215,2.00501909189412,-3.13866926264078));
#15729=CARTESIAN_POINT('Ctrl Pts',(82.6853795022768,2.09840513820848,-3.07702283230171));
#15730=CARTESIAN_POINT('Ctrl Pts',(82.6913430843387,2.1888629907155,-3.01126989331345));
#15731=CARTESIAN_POINT('Ctrl Pts',(82.6973045161068,2.27928822675991,-2.94554066291673));
#15732=CARTESIAN_POINT('Ctrl Pts',(82.7032659478749,2.36678703349163,-2.87570811134752));
#15733=CARTESIAN_POINT('Ctrl Pts',(82.7092273796431,2.45097522684397,-2.80206852162776));
#15734=CARTESIAN_POINT('Ctrl Pts',(82.7151881043369,2.53515343479185,-2.72843766616226));
#15735=CARTESIAN_POINT('Ctrl Pts',(82.7211488290308,2.61602149853302,-2.65100094352853));
#15736=CARTESIAN_POINT('Ctrl Pts',(82.7271095537246,2.69322915550566,-2.57009421586725));
#15737=CARTESIAN_POINT('Ctrl Pts',(82.7330710136579,2.77044633583596,-2.48917750857785));
#15738=CARTESIAN_POINT('Ctrl Pts',(82.7390324735912,2.84400192580809,-2.40479024528745));
#15739=CARTESIAN_POINT('Ctrl Pts',(82.7449939335244,2.9135838106701,-2.31730380845954));
#15740=CARTESIAN_POINT('Ctrl Pts',(82.750961234612,2.98323387321499,-2.22973165072083));
#15741=CARTESIAN_POINT('Ctrl Pts',(82.7569285356995,3.04890219439032,-2.13905457835484));
#15742=CARTESIAN_POINT('Ctrl Pts',(82.7628958367871,3.11031805223396,-2.04567572612267));
#15743=CARTESIAN_POINT('Ctrl Pts',(82.7688660452264,3.17176383273428,-1.95225137842023));
#15744=CARTESIAN_POINT('Ctrl Pts',(82.7748362536657,3.22895280870762,-1.85612298376126));
#15745=CARTESIAN_POINT('Ctrl Pts',(82.780806462105,3.28165950963282,-1.75771966631101));
#15746=CARTESIAN_POINT('Ctrl Pts',(82.786786148287,3.33444988277065,-1.65916013298769));
#15747=CARTESIAN_POINT('Ctrl Pts',(82.792765834469,3.38274358151401,-1.55831883405778));
#15748=CARTESIAN_POINT('Ctrl Pts',(82.798745520651,3.42636251041828,-1.45564676680166));
#15749=CARTESIAN_POINT('Ctrl Pts',(82.8042533289766,3.46653931777226,-1.3610769098518));
#15750=CARTESIAN_POINT('Ctrl Pts',(82.8097611373021,3.50275051679149,-1.26495428300126));
#15751=CARTESIAN_POINT('Ctrl Pts',(82.8152689456277,3.53489464089742,-1.16764182875346));
#15752=CARTESIAN_POINT('Ctrl Pts',(82.8212402251074,3.56974362933703,-1.06214072435452));
#15753=CARTESIAN_POINT('Ctrl Pts',(82.827211504587,3.59992020435128,-0.954912241094764));
#15754=CARTESIAN_POINT('Ctrl Pts',(82.8331827840667,3.62525361863358,-0.846406381760034));
#15755=CARTESIAN_POINT('Ctrl Pts',(82.8391466256611,3.65055547736247,-0.738035678405555));
#15756=CARTESIAN_POINT('Ctrl Pts',(82.8451104672555,3.67102607907791,-0.628391165217952));
#15757=CARTESIAN_POINT('Ctrl Pts',(82.8510743088499,3.68654393762842,-0.51793953163973));
#15758=CARTESIAN_POINT('Ctrl Pts',(82.8570323314825,3.70204665529625,-0.407595666489731));
#15759=CARTESIAN_POINT('Ctrl Pts',(82.8629903541151,3.71260618482302,-0.296446657350823));
#15760=CARTESIAN_POINT('Ctrl Pts',(82.8689483767477,3.71815190178508,-0.184970261804432));
#15761=CARTESIAN_POINT('Ctrl Pts',(82.8749024030295,3.72369389895084,-0.0735686391838515));
#15762=CARTESIAN_POINT('Ctrl Pts',(82.8808564293114,3.7242287525567,0.0381595187089541));
#15763=CARTESIAN_POINT('Ctrl Pts',(82.8868104555931,3.71973764669685,0.149731099796243));
#15764=CARTESIAN_POINT('Ctrl Pts',(82.8927623812864,3.71524812530526,0.261263318277708));
#15765=CARTESIAN_POINT('Ctrl Pts',(82.8987143069796,3.70573618642912,0.372638654563123));
#15766=CARTESIAN_POINT('Ctrl Pts',(82.9046662326728,3.69123512453875,0.483374407547002));
#15767=CARTESIAN_POINT('Ctrl Pts',(82.9106175133116,3.67673563423614,0.594098159274989));
#15768=CARTESIAN_POINT('Ctrl Pts',(82.9165687939505,3.65724815033154,0.704182053105656));
#15769=CARTESIAN_POINT('Ctrl Pts',(82.9225200745893,3.63285771524098,0.813149668458436));
#15770=CARTESIAN_POINT('Ctrl Pts',(82.9284721648498,3.60846396203706,0.922132107937947));
#15771=CARTESIAN_POINT('Ctrl Pts',(82.9344242551102,3.57916602265238,1.02999756108211));
#15772=CARTESIAN_POINT('Ctrl Pts',(82.9403763453707,3.54509964802525,1.13628167637749));
#15773=CARTESIAN_POINT('Ctrl Pts',(82.9463344547801,3.5109988232179,1.24267327322813));
#15774=CARTESIAN_POINT('Ctrl Pts',(82.9522925641894,3.47212005779636,1.34747994085396));
#15775=CARTESIAN_POINT('Ctrl Pts',(82.9582506735988,3.42864847369204,1.45025418680631));
#15776=CARTESIAN_POINT('Ctrl Pts',(82.9642117746546,3.3851550619239,1.55308003708218));
#15777=CARTESIAN_POINT('Ctrl Pts',(82.9701728757104,3.33706441541386,1.65387105651601));
#15778=CARTESIAN_POINT('Ctrl Pts',(82.9761339767663,3.28460834836788,1.7522030591036));
#15779=CARTESIAN_POINT('Ctrl Pts',(82.9821047966509,3.23206675827321,1.85069537970814));
#15780=CARTESIAN_POINT('Ctrl Pts',(82.9880756165355,3.17514573726857,1.94672031337553));
#15781=CARTESIAN_POINT('Ctrl Pts',(82.9940464364201,3.1141215448209,2.03988101775136));
#15782=CARTESIAN_POINT('Ctrl Pts',(82.9996482265334,3.0568689857869,2.12728387411033));
#15783=CARTESIAN_POINT('Ctrl Pts',(83.0052500166468,2.99600535557949,2.21216566847866));
#15784=CARTESIAN_POINT('Ctrl Pts',(83.0108518067601,2.9317903228427,2.29422602752778));
#15785=CARTESIAN_POINT('Ctrl Pts',(83.0168114313028,2.86347332463906,2.38152828624852));
#15786=CARTESIAN_POINT('Ctrl Pts',(83.0227710558454,2.79114080332129,2.46592032327333));
#15787=CARTESIAN_POINT('Ctrl Pts',(83.0287306803881,2.71506975614864,2.54701075414827));
#15788=CARTESIAN_POINT('Ctrl Pts',(83.0346826412873,2.63909653080748,2.62799690862952));
#15789=CARTESIAN_POINT('Ctrl Pts',(83.0406346021865,2.5593946229042,2.70568959725362));
#15790=CARTESIAN_POINT('Ctrl Pts',(83.0465865630856,2.47628239154729,2.77972895797645));
#15791=CARTESIAN_POINT('Ctrl Pts',(83.0525324962084,2.39325433109783,2.85369333623188));
#15792=CARTESIAN_POINT('Ctrl Pts',(83.0584784293311,2.3068231269795,2.92401146895017));
#15793=CARTESIAN_POINT('Ctrl Pts',(83.0644243624538,2.21734471882464,2.99035950353807));
#15794=CARTESIAN_POINT('Ctrl Pts',(83.0703660317093,2.12793047621776,3.0566599595192));
#15795=CARTESIAN_POINT('Ctrl Pts',(83.0763077009647,2.03547371091488,3.11899573227344));
#15796=CARTESIAN_POINT('Ctrl Pts',(83.0822493702202,1.94036369803259,3.17708298315567));
#15797=CARTESIAN_POINT('Ctrl Pts',(83.0881887801875,1.84528985022724,3.23514814666944));
#15798=CARTESIAN_POINT('Ctrl Pts',(83.0941281901548,1.74756511666116,3.28896778215306));
#15799=CARTESIAN_POINT('Ctrl Pts',(83.1000676001221,1.64760748811742,3.33830153335486));
#15800=CARTESIAN_POINT('Ctrl Pts',(83.1060062208367,1.54766314234405,3.38762872889005));
#15801=CARTESIAN_POINT('Ctrl Pts',(83.1119448415514,1.44548686641152,3.43247104061365));
#15802=CARTESIAN_POINT('Ctrl Pts',(83.1178834622661,1.34152026984447,3.47263458027136));
#15803=CARTESIAN_POINT('Ctrl Pts',(83.1238227627977,1.23754177181821,3.51280271760509));
#15804=CARTESIAN_POINT('Ctrl Pts',(83.1297620633293,1.13177293579743,3.54829086786324));
#15805=CARTESIAN_POINT('Ctrl Pts',(83.1357013638609,1.0246735800673,3.57895398361198));
#15806=CARTESIAN_POINT('Ctrl Pts',(83.1416465568446,0.917467969768757,3.60964752060936));
#15807=CARTESIAN_POINT('Ctrl Pts',(83.1475917498282,0.808929605512165,3.63550634530618));
#15808=CARTESIAN_POINT('Ctrl Pts',(83.1535369428118,0.699531761879276,3.65643581601292));
#15809=CARTESIAN_POINT('Ctrl Pts',(83.1594850391635,0.590080493200947,3.67737550774309));
#15810=CARTESIAN_POINT('Ctrl Pts',(83.1654331355152,0.479769322688583,3.69338098883143));
#15811=CARTESIAN_POINT('Ctrl Pts',(83.1713812318669,0.369078114437835,3.70440938719562));
#15812=CARTESIAN_POINT('Ctrl Pts',(83.1773390334114,0.258206297222685,3.71545578001157));
#15813=CARTESIAN_POINT('Ctrl Pts',(83.183296834956,0.146953621173151,3.72150883900468));
#15814=CARTESIAN_POINT('Ctrl Pts',(83.1892546365005,0.0358019216816396,
3.72257784134918));
#15815=CARTESIAN_POINT('Ctrl Pts',(83.1949813136312,-0.0710378061530395,
3.72360537327234));
#15816=CARTESIAN_POINT('Ctrl Pts',(83.2007079907618,-0.177783918544049,
3.72002841209837));
#15817=CARTESIAN_POINT('Ctrl Pts',(83.2064346678925,-0.284014229770194,
3.711900251864));
#15818=CARTESIAN_POINT('Ctrl Pts',(83.2124015350731,-0.394700085317414,
3.70343117783813));
#15819=CARTESIAN_POINT('Ctrl Pts',(83.2183684022538,-0.505183970064088,
3.68999341159044));
#15820=CARTESIAN_POINT('Ctrl Pts',(83.2243352694345,-0.614985652551647,
3.67160185881525));
#15821=CARTESIAN_POINT('Ctrl Pts',(83.2302951610815,-0.724658971979239,
3.65323180658485));
#15822=CARTESIAN_POINT('Ctrl Pts',(83.2362550527286,-0.833651267434829,
3.62991954790342));
#15823=CARTESIAN_POINT('Ctrl Pts',(83.2422149443756,-0.94148563776353,3.6017318551476));
#15824=CARTESIAN_POINT('Ctrl Pts',(83.2481693307303,-1.04922039894372,3.5735702000277));
#15825=CARTESIAN_POINT('Ctrl Pts',(83.2541237170851,-1.15579896101161,3.54054217004465));
#15826=CARTESIAN_POINT('Ctrl Pts',(83.2600781034398,-1.26075359887706,3.50276575371785));
#15827=CARTESIAN_POINT('Ctrl Pts',(83.2660284500849,-1.36563703104061,3.46501496652278));
#15828=CARTESIAN_POINT('Ctrl Pts',(83.27197879673,-1.46889833964291,3.42252234102821));
#15829=CARTESIAN_POINT('Ctrl Pts',(83.277929143375,-1.570084708551,3.37545575744585));
#15830=CARTESIAN_POINT('Ctrl Pts',(83.2838778657098,-1.67124345586368,3.32840202197873));
#15831=CARTESIAN_POINT('Ctrl Pts',(83.2898265880445,-1.7703280097478,3.27677698055132));
#15832=CARTESIAN_POINT('Ctrl Pts',(83.2957753103792,-1.86690579847718,3.22079653224359));
#15833=CARTESIAN_POINT('Ctrl Pts',(83.3017228809011,-1.96346488747049,3.16482692307001));
#15834=CARTESIAN_POINT('Ctrl Pts',(83.307670451423,-2.05751781852964,3.10450379698923));
#15835=CARTESIAN_POINT('Ctrl Pts',(83.3136180219449,-2.14865776894596,3.04008837938113));
#15836=CARTESIAN_POINT('Ctrl Pts',(83.3195682478411,-2.23983841004109,2.97564420262782));
#15837=CARTESIAN_POINT('Ctrl Pts',(83.3255184737372,-2.32810313115278,2.907104324154));
#15838=CARTESIAN_POINT('Ctrl Pts',(83.3314686996334,-2.41307535751767,2.83477245673105));
#15839=CARTESIAN_POINT('Ctrl Pts',(83.3364941112922,-2.48484077020848,2.77368277439161));
#15840=CARTESIAN_POINT('Ctrl Pts',(83.3415195229509,-2.55425805754174,2.70988905418821));
#15841=CARTESIAN_POINT('Ctrl Pts',(83.3465449346096,-2.62112000711956,2.64359555733806));
#15842=CARTESIAN_POINT('',(82.4430005297901,2.16151778945158,-3.03095833168065));
#15843=CARTESIAN_POINT('Origin',(82.4430005297901,0.,0.));
#15844=CARTESIAN_POINT('Ctrl Pts',(82.4430005297901,2.16151778945147,-3.03095833168073));
#15845=CARTESIAN_POINT('Ctrl Pts',(82.4497525870341,2.26438712551953,-2.9575974089732));
#15846=CARTESIAN_POINT('Ctrl Pts',(82.4565046442782,2.36346172388708,-2.87903694463822));
#15847=CARTESIAN_POINT('Ctrl Pts',(82.4632567015222,2.45826699999897,-2.79567360741844));
#15848=CARTESIAN_POINT('Ctrl Pts',(82.4700154581067,2.55316634119397,-2.71222755772141));
#15849=CARTESIAN_POINT('Ctrl Pts',(82.4767742146913,2.64378773851266,-2.62396924669582));
#15850=CARTESIAN_POINT('Ctrl Pts',(82.4835329712758,2.72969125339154,-2.53133427734421));
#15851=CARTESIAN_POINT('Ctrl Pts',(82.4902898152388,2.81557045893036,-2.43872552222812));
#15852=CARTESIAN_POINT('Ctrl Pts',(82.4970466592018,2.89673431317573,-2.3417427375673));
#15853=CARTESIAN_POINT('Ctrl Pts',(82.5038035031648,2.97278138998534,-2.24085661519358));
#15854=CARTESIAN_POINT('Ctrl Pts',(82.510548629069,3.04869658212802,-2.14014545460938));
#15855=CARTESIAN_POINT('Ctrl Pts',(82.5172937549732,3.11951259794815,-2.03554464175841));
#15856=CARTESIAN_POINT('Ctrl Pts',(82.5240388808774,3.18487011231051,-1.9275554285704));
#15857=CARTESIAN_POINT('Ctrl Pts',(82.5296232407037,3.2389802775964,-1.83815003683076));
#15858=CARTESIAN_POINT('Ctrl Pts',(82.53520760053,3.28934967007504,-1.74642274789237));
#15859=CARTESIAN_POINT('Ctrl Pts',(82.5407919603563,3.33579618241313,-1.65267401259232));
#15860=CARTESIAN_POINT('Ctrl Pts',(82.5468159793767,3.38589944983491,-1.55154439663748));
#15861=CARTESIAN_POINT('Ctrl Pts',(82.5528399983971,3.43141471863513,-1.44810467648933));
#15862=CARTESIAN_POINT('Ctrl Pts',(82.5588640174175,3.47213824854727,-1.34280435859998));
#15863=CARTESIAN_POINT('Ctrl Pts',(82.5648874941942,3.51285811278705,-1.23751351917344));
#15864=CARTESIAN_POINT('Ctrl Pts',(82.5709109709708,3.54878695248395,-1.13036279259719));
#15865=CARTESIAN_POINT('Ctrl Pts',(82.5769344477475,3.57976955737609,-1.02182066850469));
#15866=CARTESIAN_POINT('Ctrl Pts',(82.5829609225814,3.61076758319991,-0.913224519881831));
#15867=CARTESIAN_POINT('Ctrl Pts',(82.5889873974153,3.63681434419998,-0.803235978819984));
#15868=CARTESIAN_POINT('Ctrl Pts',(82.5950138722492,3.65780483342544,-0.692337607724339));
#15869=CARTESIAN_POINT('Ctrl Pts',(82.6010420246523,3.67880116570166,-0.581408366228167));
#15870=CARTESIAN_POINT('Ctrl Pts',(82.6070701770554,3.69473835749882,-0.469569189038235));
#15871=CARTESIAN_POINT('Ctrl Pts',(82.6130983294586,3.70556295161657,-0.357310472987701));
#15872=CARTESIAN_POINT('Ctrl Pts',(82.6191321312306,3.71639769015704,-0.244946552080748));
#15873=CARTESIAN_POINT('Ctrl Pts',(82.6251659330027,3.72211023554301,-0.132162710340014));
#15874=CARTESIAN_POINT('Ctrl Pts',(82.6311997347748,3.72269917905029,-0.019452115522899));
#15875=CARTESIAN_POINT('Ctrl Pts',(82.6336609534907,3.7229394121301,0.0265231146751369));
#15876=CARTESIAN_POINT('Ctrl Pts',(82.6361221722066,3.72232774982774,0.0724861757607506));
#15877=CARTESIAN_POINT('Ctrl Pts',(82.6385833909225,3.72086658053853,0.118403768231767));
#15878=CARTESIAN_POINT('Ctrl Pts',(82.6446179854142,3.71728397973704,0.230987850586364));
#15879=CARTESIAN_POINT('Ctrl Pts',(82.650652579906,3.70858350729485,0.343527835818447));
#15880=CARTESIAN_POINT('Ctrl Pts',(82.6566871743978,3.69477453776741,0.455531203723344));
#15881=CARTESIAN_POINT('Ctrl Pts',(82.6627163739924,3.68097791338929,0.56743444118052));
#15882=CARTESIAN_POINT('Ctrl Pts',(82.668745573587,3.66208193039216,0.67880161720003));
#15883=CARTESIAN_POINT('Ctrl Pts',(82.6747747731817,3.63814792340125,0.789143364637372));
#15884=CARTESIAN_POINT('Ctrl Pts',(82.6808000674154,3.61422941945254,0.899413639179759));
#15885=CARTESIAN_POINT('Ctrl Pts',(82.6868253616491,3.58527947302877,1.00865941394278));
#15886=CARTESIAN_POINT('Ctrl Pts',(82.6928506558828,3.55141075192741,1.11640012253422));
#15887=CARTESIAN_POINT('Ctrl Pts',(82.69887449913,3.5175501869521,1.22411488545155));
#15888=CARTESIAN_POINT('Ctrl Pts',(82.7048983423771,3.47877331924376,1.33032491694052));
#15889=CARTESIAN_POINT('Ctrl Pts',(82.7109221856242,3.43524298274324,1.4345637706332));
#15890=CARTESIAN_POINT('Ctrl Pts',(82.716945436337,3.39171692809766,1.53879237088688));
#15891=CARTESIAN_POINT('Ctrl Pts',(82.7229686870497,3.34343848993966,1.64104980643127));
#15892=CARTESIAN_POINT('Ctrl Pts',(82.7289919377624,3.29061879767597,1.74088928162635));
#15893=CARTESIAN_POINT('Ctrl Pts',(82.7350159406708,3.2377925091827,1.84074122497626));
#15894=CARTESIAN_POINT('Ctrl Pts',(82.7410399435792,3.18042402656934,1.93817425007928));
#15895=CARTESIAN_POINT('Ctrl Pts',(82.7470639464876,3.11877033253438,2.0327663848567));
#15896=CARTESIAN_POINT('Ctrl Pts',(82.7530900465796,3.05709517451287,2.12739145073972));
#15897=CARTESIAN_POINT('Ctrl Pts',(82.7591161466717,2.99113205645184,2.21917331991592));
#15898=CARTESIAN_POINT('Ctrl Pts',(82.7651422467637,2.92118080661426,2.30771970948997));
#15899=CARTESIAN_POINT('Ctrl Pts',(82.7711758693073,2.8511422358097,2.3963766325624));
#15900=CARTESIAN_POINT('Ctrl Pts',(82.7772094918508,2.77710583986882,2.48178969136247));
#15901=CARTESIAN_POINT('Ctrl Pts',(82.7832431143944,2.69941145893569,2.56360007369845));
#15902=CARTESIAN_POINT('Ctrl Pts',(82.7892806497584,2.62166669298755,2.64546351028742));
#15903=CARTESIAN_POINT('Ctrl Pts',(82.7953181851224,2.54025950511836,2.72371933435787));
#15904=CARTESIAN_POINT('Ctrl Pts',(82.8013557204864,2.45556495511912,2.79804723221229));
#15905=CARTESIAN_POINT('Ctrl Pts',(82.807403681777,2.37072415021567,2.87250348330291));
#15906=CARTESIAN_POINT('Ctrl Pts',(82.8134516430675,2.28258495469221,2.9430180013515));
#15907=CARTESIAN_POINT('Ctrl Pts',(82.8194996043581,2.19155420785852,3.00931183437636));
#15908=CARTESIAN_POINT('Ctrl Pts',(82.8243884869237,2.11796930713768,3.0629005974176));
#15909=CARTESIAN_POINT('Ctrl Pts',(82.8292773694893,2.04249561614066,3.11373220542137));
#15910=CARTESIAN_POINT('Ctrl Pts',(82.8341662520549,1.9653598929364,3.16168120684819));
#15911=CARTESIAN_POINT('Ctrl Pts',(82.8400765136812,1.87210907360204,3.21964765201231));
#15912=CARTESIAN_POINT('Ctrl Pts',(82.8459867753075,1.77611037840658,3.27359751554604));
#15913=CARTESIAN_POINT('Ctrl Pts',(82.8518970369338,1.67774758116333,3.32325602630923));
#15914=CARTESIAN_POINT('Ctrl Pts',(82.8577989521669,1.57952369055903,3.3728444099815));
#15915=CARTESIAN_POINT('Ctrl Pts',(82.8637008674001,1.47894270954516,3.41815329597526));
#15916=CARTESIAN_POINT('Ctrl Pts',(82.8696027826332,1.37641727118754,3.4589511499986));
#15917=CARTESIAN_POINT('Ctrl Pts',(82.875498048588,1.27400734112691,3.49970303991084));
#15918=CARTESIAN_POINT('Ctrl Pts',(82.8813933145428,1.16965770180484,3.53595384502219));
#15919=CARTESIAN_POINT('Ctrl Pts',(82.8872885804976,1.06380471935477,3.56751833654412));
#15920=CARTESIAN_POINT('Ctrl Pts',(82.8932244360264,0.957222927129104,3.59930015316592));
#15921=CARTESIAN_POINT('Ctrl Pts',(82.8991602915551,0.849117397594608,3.62633067152118));
#15922=CARTESIAN_POINT('Ctrl Pts',(82.9050961470838,0.739953470235613,3.64847042257249));
#15923=CARTESIAN_POINT('Ctrl Pts',(82.9109836667738,0.631678467811638,3.67042988900744));
#15924=CARTESIAN_POINT('Ctrl Pts',(82.9168711864638,0.522362667208827,3.68757786662143));
#15925=CARTESIAN_POINT('Ctrl Pts',(82.9227587061538,0.412473493400228,3.69982880411273));
#15926=CARTESIAN_POINT('Ctrl Pts',(82.9286450490054,0.302606285004335,3.7120772928014));
#15927=CARTESIAN_POINT('Ctrl Pts',(82.9345313918569,0.192166354445299,3.71943063976913));
#15928=CARTESIAN_POINT('Ctrl Pts',(82.9404177347085,0.0816278908404526,
3.72185497432892));
#15929=CARTESIAN_POINT('Ctrl Pts',(82.9463044212326,-0.0289170265228388,
3.72427945043284));
#15930=CARTESIAN_POINT('Ctrl Pts',(82.9521911077568,-0.139560062392199,
3.72177433367711));
#15931=CARTESIAN_POINT('Ctrl Pts',(82.9580777942809,-0.249826264947155,
3.71435787180538));
#15932=CARTESIAN_POINT('Ctrl Pts',(82.9640504041897,-0.361701937499702,
3.70683315760796));
#15933=CARTESIAN_POINT('Ctrl Pts',(82.9700230140986,-0.473189236914967,
3.69425260232078));
#15934=CARTESIAN_POINT('Ctrl Pts',(82.9759956240075,-0.583798126309067,
3.67668972177665));
#15935=CARTESIAN_POINT('Ctrl Pts',(82.9818907079216,-0.692971284204131,
3.65935481188613));
#15936=CARTESIAN_POINT('Ctrl Pts',(82.9877857918357,-0.801288292914002,
3.63716630404435));
#15937=CARTESIAN_POINT('Ctrl Pts',(82.9936808757498,-0.908290114054953,
3.61024606241874));
#15938=CARTESIAN_POINT('Ctrl Pts',(82.999692248656,-1.01740269971021,3.58279478038529));
#15939=CARTESIAN_POINT('Ctrl Pts',(83.0057036215623,-1.12514721360662,3.55042324853487));
#15940=CARTESIAN_POINT('Ctrl Pts',(83.0117149944685,-1.23105640664389,3.51331292175363));
#15941=CARTESIAN_POINT('Ctrl Pts',(83.0177263673747,-1.33696559968117,3.47620259497239));
#15942=CARTESIAN_POINT('Ctrl Pts',(83.023737740281,-1.44103906794508,3.43435370796953));
#15943=CARTESIAN_POINT('Ctrl Pts',(83.0297491131872,-1.542835502784,3.38799736922112));
#15944=CARTESIAN_POINT('Ctrl Pts',(83.0357287047233,-1.64409375271539,3.34188611058699));
#15945=CARTESIAN_POINT('Ctrl Pts',(83.0417082962595,-1.74343945101141,3.29116017750618));
#15946=CARTESIAN_POINT('Ctrl Pts',(83.0476878877956,-1.84042560292446,3.23600079768225));
#15947=CARTESIAN_POINT('Ctrl Pts',(83.0536609650252,-1.93730609586108,3.18090150977348));
#15948=CARTESIAN_POINT('Ctrl Pts',(83.0596340422548,-2.03183179406103,3.1213785772606));
#15949=CARTESIAN_POINT('Ctrl Pts',(83.0656071194844,-2.12357676031699,3.05766075710527));
#15950=CARTESIAN_POINT('Ctrl Pts',(83.0715742291671,-2.21523006655029,2.99400659577591));
#15951=CARTESIAN_POINT('Ctrl Pts',(83.0775413388497,-2.30410782960365,2.9261661202019));
#15952=CARTESIAN_POINT('Ctrl Pts',(83.0835084485324,-2.3898105926219,2.85441288076763));
#15953=CARTESIAN_POINT('Ctrl Pts',(83.0890762444753,-2.46977820200121,2.78746130510422));
#15954=CARTESIAN_POINT('Ctrl Pts',(83.0946440404181,-2.54698154549054,2.71710370215753));
#15955=CARTESIAN_POINT('Ctrl Pts',(83.100211836361,-2.62112000711957,2.64359555733806));
#15956=CARTESIAN_POINT('Origin',(80.1322559480305,0.,0.));
#15957=CARTESIAN_POINT('',(84.5967274725783,-2.62112000711956,2.64359555733807));
#15958=CARTESIAN_POINT('',(84.3497092113127,-2.62112002533987,2.64359553927266));
#15959=CARTESIAN_POINT('',(80.1322559480305,-2.62112000711956,2.64359555733806));
#15960=CARTESIAN_POINT('',(83.5037451115797,-3.72274997864689,-0.000398728739238651));
#15961=CARTESIAN_POINT('Ctrl Pts',(83.5037451115797,-3.72274997864689,-0.00039872873923823));
#15962=CARTESIAN_POINT('Ctrl Pts',(83.5100196206599,-3.72273733869349,-0.118412259214994));
#15963=CARTESIAN_POINT('Ctrl Pts',(83.51629412974,-3.71710876285587,-0.236304017798562));
#15964=CARTESIAN_POINT('Ctrl Pts',(83.5225686388201,-3.70592449650868,-0.353540929281022));
#15965=CARTESIAN_POINT('Ctrl Pts',(83.5288611095432,-3.69470821366485,-0.471113447504741));
#15966=CARTESIAN_POINT('Ctrl Pts',(83.5351535802664,-3.67790446628232,-0.588027026941602));
#15967=CARTESIAN_POINT('Ctrl Pts',(83.5414460509894,-3.65562518860896,-0.703755669893829));
#15968=CARTESIAN_POINT('Ctrl Pts',(83.5477474655781,-3.63331424406364,-0.819648804898809));
#15969=CARTESIAN_POINT('Ctrl Pts',(83.5540488801668,-3.60551231776947,-0.934353309309916));
#15970=CARTESIAN_POINT('Ctrl Pts',(83.5603502947555,-3.57238150868199,-1.04735758885255));
#15971=CARTESIAN_POINT('Ctrl Pts',(83.5666688213221,-3.53916073032393,-1.16066874024292));
#15972=CARTESIAN_POINT('Ctrl Pts',(83.5729873478887,-3.5005822350553,-1.2722701059141));
#15973=CARTESIAN_POINT('Ctrl Pts',(83.5793058744553,-3.4568573355477,-1.38166744340672));
#15974=CARTESIAN_POINT('Ctrl Pts',(83.5854040463559,-3.41465731458977,-1.4872496171091));
#15975=CARTESIAN_POINT('Ctrl Pts',(83.5915022182565,-3.36766400046035,-1.59077869702065));
#15976=CARTESIAN_POINT('Ctrl Pts',(83.5976003901571,-3.31610731420533,-1.69183327877598));
#15977=CARTESIAN_POINT('Ctrl Pts',(83.6035656848774,-3.26567403135889,-1.79068591409443));
#15978=CARTESIAN_POINT('Ctrl Pts',(83.6095309795976,-3.21073524337409,-1.88744121534554));
#15979=CARTESIAN_POINT('Ctrl Pts',(83.6154962743178,-3.15148926053915,-1.98166167728158));
#15980=CARTESIAN_POINT('Ctrl Pts',(83.6214539899425,-3.09231855159846,-2.07576242914194));
#15981=CARTESIAN_POINT('Ctrl Pts',(83.6274117055672,-3.02885175060343,-2.16733439615148));
#15982=CARTESIAN_POINT('Ctrl Pts',(83.6333694211919,-2.96133374140531,-2.25596321656946));
#15983=CARTESIAN_POINT('Ctrl Pts',(83.6393211856149,-2.89388317639428,-2.34450350507104));
#15984=CARTESIAN_POINT('Ctrl Pts',(83.645272950038,-2.82238970387071,-2.43010616471014));
#15985=CARTESIAN_POINT('Ctrl Pts',(83.6512247144611,-2.74714192160807,-2.51238508693303));
#15986=CARTESIAN_POINT('Ctrl Pts',(83.6571723075251,-2.67194687757433,-2.59460634307591));
#15987=CARTESIAN_POINT('Ctrl Pts',(83.6631199005891,-2.59300303846704,-2.67350818876696));
#15988=CARTESIAN_POINT('Ctrl Pts',(83.6690674936532,-2.51063931632746,-2.74873748943233));
#15989=CARTESIAN_POINT('Ctrl Pts',(83.6750128818184,-2.42830612816521,-2.82393890100162));
#15990=CARTESIAN_POINT('Ctrl Pts',(83.6809582699837,-2.34255588496676,-2.89547019330391));
#15991=CARTESIAN_POINT('Ctrl Pts',(83.6869036581489,-2.25375393754337,-2.96301548283295));
#15992=CARTESIAN_POINT('Ctrl Pts',(83.6928483045751,-2.16496306893846,-3.03055234549722));
#15993=CARTESIAN_POINT('Ctrl Pts',(83.6987929510012,-2.07312158516433,-3.0941039419349));
#15994=CARTESIAN_POINT('Ctrl Pts',(83.7047375974274,-1.97862684690804,-3.15339552913915));
#15995=CARTESIAN_POINT('Ctrl Pts',(83.7106829643435,-1.88412065590747,-3.21269430247247));
#15996=CARTESIAN_POINT('Ctrl Pts',(83.7166283312597,-1.78696092457647,-3.26773181874748));
#15997=CARTESIAN_POINT('Ctrl Pts',(83.7225736981759,-1.68757217285197,-3.31827782500436));
#15998=CARTESIAN_POINT('Ctrl Pts',(83.7285249846558,-1.58808446372736,-3.36887415789559));
#15999=CARTESIAN_POINT('Ctrl Pts',(83.7344762711357,-1.48636367330883,-3.41496985803524));
#16000=CARTESIAN_POINT('Ctrl Pts',(83.7404275576156,-1.3828571226216,-3.45638159654207));
#16001=CARTESIAN_POINT('Ctrl Pts',(83.7463817713833,-1.27929965967314,-3.49781370443842));
#16002=CARTESIAN_POINT('Ctrl Pts',(83.7523359851509,-1.17395508017414,-3.53455712242865));
#16003=CARTESIAN_POINT('Ctrl Pts',(83.7582901989185,-1.0672870366516,-3.56647808683797));
#16004=CARTESIAN_POINT('Ctrl Pts',(83.7642540941447,-0.960445552555769,
-3.59845095423703));
#16005=CARTESIAN_POINT('Ctrl Pts',(83.770217989371,-0.852276709261824,-3.62558559676572));
#16006=CARTESIAN_POINT('Ctrl Pts',(83.7761818845972,-0.743256032909034,
-3.64779906684076));
#16007=CARTESIAN_POINT('Ctrl Pts',(83.781849006828,-0.63966040033416,-3.66890715900358));
#16008=CARTESIAN_POINT('Ctrl Pts',(83.7875161290588,-0.535295977888283,
-3.68557203647516));
#16009=CARTESIAN_POINT('Ctrl Pts',(83.7931832512895,-0.430573663541631,
-3.69776606652778));
#16010=CARTESIAN_POINT('Ctrl Pts',(83.7991495636772,-0.320322637374219,
-3.71060386843089));
#16011=CARTESIAN_POINT('Ctrl Pts',(83.805115876065,-0.209319446371947,-3.71852726417688));
#16012=CARTESIAN_POINT('Ctrl Pts',(83.8110821884527,-0.0980383235348542,
-3.72145886039581));
#16013=CARTESIAN_POINT('Ctrl Pts',(83.8170409367009,0.013101716186779,-3.72438673991313));
#16014=CARTESIAN_POINT('Ctrl Pts',(83.8229996849491,0.124518573731149,-3.72233539448482));
#16015=CARTESIAN_POINT('Ctrl Pts',(83.8289584331973,0.2357314749135,-3.71527902508481));
#16016=CARTESIAN_POINT('Ctrl Pts',(83.8349112437453,0.346833556029731,-3.70822968712912));
#16017=CARTESIAN_POINT('Ctrl Pts',(83.8408640542932,0.457731671199903,-3.69618527171105));
#16018=CARTESIAN_POINT('Ctrl Pts',(83.8468168648411,0.567944340902615,-3.67917202480894));
#16019=CARTESIAN_POINT('Ctrl Pts',(83.8527655202028,0.678080079856902,-3.66217065350897));
#16020=CARTESIAN_POINT('Ctrl Pts',(83.8587141755644,0.787530914333091,-3.64020741337706));
#16021=CARTESIAN_POINT('Ctrl Pts',(83.8646628309261,0.895820469822217,-3.61336038174267));
#16022=CARTESIAN_POINT('Ctrl Pts',(83.8706092908679,1.00407005980229,-3.58652325831485));
#16023=CARTESIAN_POINT('Ctrl Pts',(83.8765557508097,1.11115881871125,-3.5548060268469));
#16024=CARTESIAN_POINT('Ctrl Pts',(83.8825022107516,1.21662118406317,-3.5183377406083));
#16025=CARTESIAN_POINT('Ctrl Pts',(83.8884479371757,1.32207054024423,-3.48187395286702));
#16026=CARTESIAN_POINT('Ctrl Pts',(83.8943936635997,1.42589350793631,-3.44066041211545));
#16027=CARTESIAN_POINT('Ctrl Pts',(83.9003393900238,1.52764102649755,-3.39487561725927));
#16028=CARTESIAN_POINT('Ctrl Pts',(83.9062858439079,1.62940099387302,-3.34908522063104));
#16029=CARTESIAN_POINT('Ctrl Pts',(83.9122322977919,1.72908462725492,-3.29872262936565));
#16030=CARTESIAN_POINT('Ctrl Pts',(83.918178751676,1.82626484219466,-3.24401360796525));
#16031=CARTESIAN_POINT('Ctrl Pts',(83.9241311294265,1.92354186821385,-3.18925008535366));
#16032=CARTESIAN_POINT('Ctrl Pts',(83.930083507177,2.01831012997369,-3.130131688067));
#16033=CARTESIAN_POINT('Ctrl Pts',(83.9360358849275,2.11016895898102,-3.06692916890054));
#16034=CARTESIAN_POINT('Ctrl Pts',(83.9419911939282,2.20207302389456,-3.00369552563572));
#16035=CARTESIAN_POINT('Ctrl Pts',(83.9479465029288,2.29106446846605,-2.93637400447061));
#16036=CARTESIAN_POINT('Ctrl Pts',(83.9539018119295,2.3767748226723,-2.86527642729477));
#16037=CARTESIAN_POINT('Ctrl Pts',(83.9598667975774,2.46262444570119,-2.7940633252683));
#16038=CARTESIAN_POINT('Ctrl Pts',(83.9658317832255,2.54518201527315,-2.71906218676769));
#16039=CARTESIAN_POINT('Ctrl Pts',(83.9717967688734,2.62411477163207,-2.64062288632859));
#16040=CARTESIAN_POINT('Ctrl Pts',(83.9774532167229,2.69896474551428,-2.56624084444844));
#16041=CARTESIAN_POINT('Ctrl Pts',(83.9831096645724,2.77055530768488,-2.48876764338392));
#16042=CARTESIAN_POINT('Ctrl Pts',(83.9887661124219,2.83863709197814,-2.40852797836062));
#16043=CARTESIAN_POINT('Ctrl Pts',(83.9947321230154,2.91044481603531,-2.32389700424257));
#16044=CARTESIAN_POINT('Ctrl Pts',(84.0006981336089,2.97858019832519,-2.23591555189983));
#16045=CARTESIAN_POINT('Ctrl Pts',(84.0066641442025,3.04271589798734,-2.14493531991878));
#16046=CARTESIAN_POINT('Ctrl Pts',(84.0126225879999,3.10677025321431,-2.0540704797651));
#16047=CARTESIAN_POINT('Ctrl Pts',(84.0185810317973,3.1668347757237,-1.9602147615424));
#16048=CARTESIAN_POINT('Ctrl Pts',(84.0245394755947,3.22262143274553,-1.86375391715461));
#16049=CARTESIAN_POINT('Ctrl Pts',(84.0304919794575,3.27835247640454,-1.76738923396779));
#16050=CARTESIAN_POINT('Ctrl Pts',(84.0364444833203,3.32981392953477,-1.66842494932434));
#16051=CARTESIAN_POINT('Ctrl Pts',(84.0423969871831,3.37676067896021,-1.56727626139369));
#16052=CARTESIAN_POINT('Ctrl Pts',(84.0483453337523,3.42367464026426,-1.46619821680893));
#16053=CARTESIAN_POINT('Ctrl Pts',(84.0542936803215,3.46607999504213,-1.3629391807151));
#16054=CARTESIAN_POINT('Ctrl Pts',(84.0602420268907,3.50377759415442,-1.25793884318811));
#16055=CARTESIAN_POINT('Ctrl Pts',(84.0661881768666,3.54146127237411,-1.15297727997188));
#16056=CARTESIAN_POINT('Ctrl Pts',(84.0721343268425,3.57444051035109,-1.04627608558645));
#16057=CARTESIAN_POINT('Ctrl Pts',(84.0780804768184,3.60256457584799,-0.938294217900349));
#16058=CARTESIAN_POINT('Ctrl Pts',(84.084025892473,3.63068516815607,-0.830325685463184));
#16059=CARTESIAN_POINT('Ctrl Pts',(84.0899713081276,3.65395167536634,-0.721077197666321));
#16060=CARTESIAN_POINT('Ctrl Pts',(84.0959167237821,3.67226366375991,-0.61102139596633));
#16061=CARTESIAN_POINT('Ctrl Pts',(84.1018628664623,3.69057789140544,-0.500952136270207));
#16062=CARTESIAN_POINT('Ctrl Pts',(84.1078090091424,3.70393632765888,-0.390075777745001));
#16063=CARTESIAN_POINT('Ctrl Pts',(84.1137551518225,3.71229005859827,-0.278872880238347));
#16064=CARTESIAN_POINT('Ctrl Pts',(84.1197072196245,3.72065211373654,-0.167559172958134));
#16065=CARTESIAN_POINT('Ctrl Pts',(84.1256592874266,3.72399947021162,-0.0559186932835599));
#16066=CARTESIAN_POINT('Ctrl Pts',(84.1316113552286,3.72233530045396,0.0555650384174694));
#16067=CARTESIAN_POINT('Ctrl Pts',(84.1375663545071,3.72067031106946,0.167103677412746));
#16068=CARTESIAN_POINT('Ctrl Pts',(84.1435213537856,3.7139889021167,0.278484998212509));
#16069=CARTESIAN_POINT('Ctrl Pts',(84.1494763530642,3.70234627688846,0.38922950621725));
#16070=CARTESIAN_POINT('Ctrl Pts',(84.1554410326672,3.69068472564788,0.500154038218728));
#16071=CARTESIAN_POINT('Ctrl Pts',(84.1614057122701,3.67404590390891,0.610439275807124));
#16072=CARTESIAN_POINT('Ctrl Pts',(84.1673703918731,3.65253648259817,0.719614345180374));
#16073=CARTESIAN_POINT('Ctrl Pts',(84.1730299191002,3.63212748100068,0.823204029582159));
#16074=CARTESIAN_POINT('Ctrl Pts',(84.1786894463272,3.60733398724194,0.925794034213578));
#16075=CARTESIAN_POINT('Ctrl Pts',(84.1843489735542,3.57828820258272,1.02699615469453));
#16076=CARTESIAN_POINT('Ctrl Pts',(84.1903149038667,3.54766989822665,1.1336772914832));
#16077=CARTESIAN_POINT('Ctrl Pts',(84.1962808341792,3.51222729159586,1.23915996827174));
#16078=CARTESIAN_POINT('Ctrl Pts',(84.2022467644917,3.47207156306853,1.34297677695144));
#16079=CARTESIAN_POINT('Ctrl Pts',(84.2082051258581,3.4319667799146,1.44666187376142));
#16080=CARTESIAN_POINT('Ctrl Pts',(84.2141634872244,3.38716091515584,1.54868491978055));
#16081=CARTESIAN_POINT('Ctrl Pts',(84.2201218485908,3.33781528368355,1.64859233727095));
#16082=CARTESIAN_POINT('Ctrl Pts',(84.2260742679927,3.28851886204741,1.74840012228129));
#16083=CARTESIAN_POINT('Ctrl Pts',(84.2320266873946,3.23469186245655,1.84609610348638));
#16084=CARTESIAN_POINT('Ctrl Pts',(84.2379791067965,3.17654390277376,1.94124609368592));
#16085=CARTESIAN_POINT('Ctrl Pts',(84.2439273661645,3.11843658160552,2.03632958534823));
#16086=CARTESIAN_POINT('Ctrl Pts',(84.2498756255326,3.05601452415942,2.12887027078323));
#16087=CARTESIAN_POINT('Ctrl Pts',(84.2558238849006,2.98953321612768,2.21845863431557));
#16088=CARTESIAN_POINT('Ctrl Pts',(84.2617699460361,2.92307647685909,2.30801388966532));
#16089=CARTESIAN_POINT('Ctrl Pts',(84.2677160071716,2.85256371746134,2.39461865776034));
#16090=CARTESIAN_POINT('Ctrl Pts',(84.273662068307,2.77829330399252,2.47789303229384));
#16091=CARTESIAN_POINT('Ctrl Pts',(84.2796073935833,2.7040320819134,2.5611571011458));
#16092=CARTESIAN_POINT('Ctrl Pts',(84.2855527188597,2.62601440807823,2.64109128500481));
#16093=CARTESIAN_POINT('Ctrl Pts',(84.291498044136,2.54457792489982,2.71734994923593));
#16094=CARTESIAN_POINT('Ctrl Pts',(84.2974440950003,2.46313150293226,2.79361792033734));
#16095=CARTESIAN_POINT('Ctrl Pts',(84.3033901458646,2.37826574669442,2.86620919527541));
#16096=CARTESIAN_POINT('Ctrl Pts',(84.3093361967289,2.2903534541501,2.9348166241799));
#16097=CARTESIAN_POINT('Ctrl Pts',(84.3152881710003,2.20235358410068,3.0034923992426));
#16098=CARTESIAN_POINT('Ctrl Pts',(84.3212401452717,2.1113014445005,3.06817614342487));
#16099=CARTESIAN_POINT('Ctrl Pts',(84.3271921195431,2.01760117679494,3.12860241224348));
#16100=CARTESIAN_POINT('Ctrl Pts',(84.3331470242174,1.92385477657584,3.18905843141106));
#16101=CARTESIAN_POINT('Ctrl Pts',(84.3391019288917,1.82745801067643,3.24525258830528));
#16102=CARTESIAN_POINT('Ctrl Pts',(84.345056833566,1.72884051915109,3.2969649712791));
#16103=CARTESIAN_POINT('Ctrl Pts',(84.3510214177228,1.63006272845468,3.34876141086394));
#16104=CARTESIAN_POINT('Ctrl Pts',(84.3569860018796,1.52905737681446,3.39606134140062));
#16105=CARTESIAN_POINT('Ctrl Pts',(84.3629505860364,1.42627546643135,3.43869246318365));
#16106=CARTESIAN_POINT('Ctrl Pts',(84.3686110022531,1.32873498799592,3.47914958252942));
#16107=CARTESIAN_POINT('Ctrl Pts',(84.3742714184699,1.22959496450997,3.51540223207884));
#16108=CARTESIAN_POINT('Ctrl Pts',(84.3799318346867,1.12925196292743,3.54734514344524));
#16109=CARTESIAN_POINT('Ctrl Pts',(84.3858978809983,1.0234910132782,3.5810127892939));
#16110=CARTESIAN_POINT('Ctrl Pts',(84.39186392731,0.91605267053247,3.61000083033015));
#16111=CARTESIAN_POINT('Ctrl Pts',(84.3978299736217,0.807387589059532,3.63414265591386));
#16112=CARTESIAN_POINT('Ctrl Pts',(84.4037884527917,0.698860334888818,3.65825386078072));
#16113=CARTESIAN_POINT('Ctrl Pts',(84.4097469319616,0.589109839862022,3.67753098430548));
#16114=CARTESIAN_POINT('Ctrl Pts',(84.4157054111316,0.478603042662136,3.6918568079023));
#16115=CARTESIAN_POINT('Ctrl Pts',(84.4216579499752,0.368206415596873,3.70616834931961));
#16116=CARTESIAN_POINT('Ctrl Pts',(84.4276104888187,0.257055397390509,3.71553835602055));
#16117=CARTESIAN_POINT('Ctrl Pts',(84.4335630276622,0.145627568430018,3.71990055966731));
#16118=CARTESIAN_POINT('Ctrl Pts',(84.4395114084652,0.0342775754051283,
3.724259716174));
#16119=CARTESIAN_POINT('Ctrl Pts',(84.4454597892681,-0.077348428395596,
3.72361801180684));
#16120=CARTESIAN_POINT('Ctrl Pts',(84.4514081700711,-0.188767965640915,
3.71796102960316));
#16121=CARTESIAN_POINT('Ctrl Pts',(84.4573543538131,-0.300146349583368,
3.71230613683108));
#16122=CARTESIAN_POINT('Ctrl Pts',(84.4633005375551,-0.411318002711453,
3.70163966999279));
#16123=CARTESIAN_POINT('Ctrl Pts',(84.4692467212971,-0.52180131642087,3.68599931479666));
#16124=CARTESIAN_POINT('Ctrl Pts',(84.4751921702078,-0.632270976566676,
3.67036089244068));
#16125=CARTESIAN_POINT('Ctrl Pts',(84.4811376191185,-0.742052053729621,
3.6497498626038));
#16126=CARTESIAN_POINT('Ctrl Pts',(84.4870830680292,-0.850669686046545,
3.62425559911846));
#16127=CARTESIAN_POINT('Ctrl Pts',(84.4930292434128,-0.959300590324678,
3.59875822049546));
#16128=CARTESIAN_POINT('Ctrl Pts',(84.4989754187964,-1.06676736130999,3.56837651758695));
#16129=CARTESIAN_POINT('Ctrl Pts',(84.50492159418,-1.17260767456877,3.53325045871962));
#16130=CARTESIAN_POINT('Ctrl Pts',(84.510873693601,-1.2785534340902,3.4980894045701));
#16131=CARTESIAN_POINT('Ctrl Pts',(84.516825793022,-1.38286910249047,3.45817468400298));
#16132=CARTESIAN_POINT('Ctrl Pts',(84.522777892443,-1.48510968634047,3.41369547294976));
#16133=CARTESIAN_POINT('Ctrl Pts',(84.5287329227958,-1.58740061548134,3.36919435945102));
#16134=CARTESIAN_POINT('Ctrl Pts',(84.5346879531485,-1.68761404933881,3.32012446016647));
#16135=CARTESIAN_POINT('Ctrl Pts',(84.5406429835013,-1.78532875113122,3.26672141647926));
#16136=CARTESIAN_POINT('Ctrl Pts',(84.5466076929119,-1.88320227432364,3.2132315737126));
#16137=CARTESIAN_POINT('Ctrl Pts',(84.5525724023226,-1.97856859235349,3.15539472877556));
#16138=CARTESIAN_POINT('Ctrl Pts',(84.5585371117333,-2.07103424867934,3.09349069875718));
#16139=CARTESIAN_POINT('Ctrl Pts',(84.5641963064285,-2.1587637784421,3.03475741702073));
#16140=CARTESIAN_POINT('Ctrl Pts',(84.5698555011238,-2.24388219142092,2.97236346029204));
#16141=CARTESIAN_POINT('Ctrl Pts',(84.575514695819,-2.32608221373895,2.90658030981897));
#16142=CARTESIAN_POINT('Ctrl Pts',(84.581413414995,-2.41176133842471,2.83801289836744));
#16143=CARTESIAN_POINT('Ctrl Pts',(84.587312134171,-2.49455984951417,2.76553054908317));
#16144=CARTESIAN_POINT('Ctrl Pts',(84.5932108533469,-2.57409385340434,2.68940669969531));
#16145=CARTESIAN_POINT('Ctrl Pts',(84.5943830597574,-2.58989902507423,2.67427920140653));
#16146=CARTESIAN_POINT('Ctrl Pts',(84.5955552661679,-2.60557536834159,2.65900803735653));
#16147=CARTESIAN_POINT('Ctrl Pts',(84.5967274725783,-2.62112000711956,2.64359555733807));
#16148=CARTESIAN_POINT('Ctrl Pts',(83.3465449346096,-2.62112000711956,2.64359555733806));
#16149=CARTESIAN_POINT('Ctrl Pts',(83.3525016691969,-2.70037299466952,2.56501636971816));
#16150=CARTESIAN_POINT('Ctrl Pts',(83.3584584037842,-2.77603460091793,2.48292445303177));
#16151=CARTESIAN_POINT('Ctrl Pts',(83.3644151383715,-2.84779618052708,2.39769148905262));
#16152=CARTESIAN_POINT('Ctrl Pts',(83.3706822034804,-2.9232963535055,2.30801810729406));
#16153=CARTESIAN_POINT('Ctrl Pts',(83.3769492685892,-2.99447886170437,2.21486800490521));
#16154=CARTESIAN_POINT('Ctrl Pts',(83.3832163336981,-3.0610357268376,2.1187090035028));
#16155=CARTESIAN_POINT('Ctrl Pts',(83.389483398807,-3.12759259197083,2.02255000210039));
#16156=CARTESIAN_POINT('Ctrl Pts',(83.3957504639159,-3.18952359244235,1.92338258779279));
#16157=CARTESIAN_POINT('Ctrl Pts',(83.4020175290247,-3.24657727312924,1.82170348083895));
#16158=CARTESIAN_POINT('Ctrl Pts',(83.4082277166816,-3.30311315674049,1.72094717401999));
#16159=CARTESIAN_POINT('Ctrl Pts',(83.4144379043384,-3.35502911036208,1.61742461319456));
#16160=CARTESIAN_POINT('Ctrl Pts',(83.4206480919953,-3.40205797839426,1.51157833873867));
#16161=CARTESIAN_POINT('Ctrl Pts',(83.4268480740761,-3.44900956105002,1.40590600785203));
#16162=CARTESIAN_POINT('Ctrl Pts',(83.4330480561568,-3.49108990258534,1.29791790193999));
#16163=CARTESIAN_POINT('Ctrl Pts',(83.4392480382376,-3.52807725450457,1.18808183587979));
#16164=CARTESIAN_POINT('Ctrl Pts',(83.445435562709,-3.56499028782464,1.07846646316866));
#16165=CARTESIAN_POINT('Ctrl Pts',(83.4516230871803,-3.59683061192906,0.96701087846192));
#16166=CARTESIAN_POINT('Ctrl Pts',(83.4578106116517,-3.62342453387416,0.854202674907337));
#16167=CARTESIAN_POINT('Ctrl Pts',(83.463990675881,-3.64998639176911,0.741530483179206));
#16168=CARTESIAN_POINT('Ctrl Pts',(83.4701707401103,-3.67131435686101,0.627509275877126));
#16169=CARTESIAN_POINT('Ctrl Pts',(83.4763508043396,-3.68728427496461,0.512642407628058));
#16170=CARTESIAN_POINT('Ctrl Pts',(83.482522178374,-3.70323173671555,0.397937061240715));
#16171=CARTESIAN_POINT('Ctrl Pts',(83.4886935524083,-3.71383611662847,0.282388787199165));
#16172=CARTESIAN_POINT('Ctrl Pts',(83.4948649264427,-3.71902428479849,0.166511055425917));
#16173=CARTESIAN_POINT('Ctrl Pts',(83.497824988145,-3.72151275783868,0.110931012137859));
#16174=CARTESIAN_POINT('Ctrl Pts',(83.5007850498474,-3.72275594166151,0.0552753217717917));
#16175=CARTESIAN_POINT('Ctrl Pts',(83.5037451115497,-3.72274997864695,-0.000398728175137864));
#16176=CARTESIAN_POINT('',(83.2572559480305,-3.72274911375701,0.00256875873404117));
#16177=CARTESIAN_POINT('Ctrl Pts',(83.100211836361,-2.62112000711957,2.64359555733806));
#16178=CARTESIAN_POINT('Ctrl Pts',(83.1061733650853,-2.70050125117219,2.56488920363776));
#16179=CARTESIAN_POINT('Ctrl Pts',(83.1121348938096,-2.77636815978871,2.48257080322071));
#16180=CARTESIAN_POINT('Ctrl Pts',(83.1180964225339,-2.84838564888578,2.39699118849476));
#16181=CARTESIAN_POINT('Ctrl Pts',(83.124057147844,-2.92039343244001,2.31142310703146));
#16182=CARTESIAN_POINT('Ctrl Pts',(83.1300178731541,-2.98855256152826,2.22259500245706));
#16183=CARTESIAN_POINT('Ctrl Pts',(83.1359785984642,-3.05256744398181,2.13089172940399));
#16184=CARTESIAN_POINT('Ctrl Pts',(83.1419399627032,-3.11658918817695,2.03917862669667));
#16185=CARTESIAN_POINT('Ctrl Pts',(83.1479013269421,-3.17646556556848,1.94459008277441));
#16186=CARTESIAN_POINT('Ctrl Pts',(83.1538626911811,-3.23194404411675,1.84754032654183));
#16187=CARTESIAN_POINT('Ctrl Pts',(83.1598298427706,-3.2874763817128,1.75039635345986));
#16188=CARTESIAN_POINT('Ctrl Pts',(83.1657969943601,-3.3386020847474,1.65078675510819));
#16189=CARTESIAN_POINT('Ctrl Pts',(83.1717641459496,-3.3851143192338,1.54915093138736));
#16190=CARTESIAN_POINT('Ctrl Pts',(83.1777341182834,-3.43164854061269,1.44746706319059));
#16191=CARTESIAN_POINT('Ctrl Pts',(83.1837040906172,-3.47356479129552,1.34375544507299));
#16192=CARTESIAN_POINT('Ctrl Pts',(83.189674062951,-3.51070488846345,1.23847436332724));
#16193=CARTESIAN_POINT('Ctrl Pts',(83.1956536293093,-3.54790467150296,1.13302408996371));
#16194=CARTESIAN_POINT('Ctrl Pts',(83.2016331956676,-3.58031284013752,1.02599970947008));
#16195=CARTESIAN_POINT('Ctrl Pts',(83.2076127620259,-3.60782133468535,0.917874054263007));
#16196=CARTESIAN_POINT('Ctrl Pts',(83.2135191661238,-3.63499325237795,0.811071357422008));
#16197=CARTESIAN_POINT('Ctrl Pts',(83.2194255702217,-3.65738473422337,0.703194579387955));
#16198=CARTESIAN_POINT('Ctrl Pts',(83.2253319743196,-3.67494124204485,0.594705330409806));
#16199=CARTESIAN_POINT('Ctrl Pts',(83.2345685167955,-3.70239642925054,0.42504786374353));
#16200=CARTESIAN_POINT('Ctrl Pts',(83.2438050592713,-3.71810656497179,0.253443539326488));
#16201=CARTESIAN_POINT('Ctrl Pts',(83.2530416017472,-3.72186436816731,0.0811984449760008));
#16202=CARTESIAN_POINT('Ctrl Pts',(83.2544463838416,-3.72243589097006,0.0550017566555983));
#16203=CARTESIAN_POINT('Ctrl Pts',(83.2558511659361,-3.72273102045438,0.0287903051327956));
#16204=CARTESIAN_POINT('Ctrl Pts',(83.2572559480305,-3.72274911375701,0.00256875873404105));
#16205=CARTESIAN_POINT('Ctrl Pts',(83.2585049200401,-3.72274907161456,0.00262912398830983));
#16206=CARTESIAN_POINT('Ctrl Pts',(83.2638576126972,-3.72282728496551,-0.108118288811131));
#16207=CARTESIAN_POINT('Ctrl Pts',(83.2691451236267,-3.71796356302337,-0.218816680367323));
#16208=CARTESIAN_POINT('Ctrl Pts',(83.2833777464751,-3.69177043663755,-0.513918430758105));
#16209=CARTESIAN_POINT('Ctrl Pts',(83.2923742746305,-3.66158130974653,-0.697205937793369));
#16210=CARTESIAN_POINT('Ctrl Pts',(83.3051807990402,-3.6019411919301,-0.943105964834372));
#16211=CARTESIAN_POINT('Ctrl Pts',(83.3086466220414,-3.5842391240922,-1.00829480213931));
#16212=CARTESIAN_POINT('Ctrl Pts',(83.3145392556633,-3.55165987094859,-1.11653489041305));
#16213=CARTESIAN_POINT('Ctrl Pts',(83.316935558106,-3.53774802543589,-1.15986062570442));
#16214=CARTESIAN_POINT('Ctrl Pts',(83.3215329364804,-3.50983776513739,-1.24160270923904));
#16215=CARTESIAN_POINT('Ctrl Pts',(83.3237287763499,-3.49599373319366,-1.28006486725557));
#16216=CARTESIAN_POINT('Ctrl Pts',(83.3295758461878,-3.4578068614688,-1.38091393073346));
#16217=CARTESIAN_POINT('Ctrl Pts',(83.3332605728359,-3.43240997422359,-1.44288342070459));
#16218=CARTESIAN_POINT('Ctrl Pts',(83.3515733136363,-3.29981066759159,-1.74308846907473));
#16219=CARTESIAN_POINT('Ctrl Pts',(83.3669542903669,-3.16941840436925,-1.97024382688032));
#16220=CARTESIAN_POINT('Ctrl Pts',(83.3897565217143,-2.94335362567548,-2.28277272151319));
#16221=CARTESIAN_POINT('Ctrl Pts',(83.3971055115402,-2.8653311137376,-2.37997095737977));
#16222=CARTESIAN_POINT('Ctrl Pts',(83.4086512496694,-2.7323903958003,-2.52954903307825));
#16223=CARTESIAN_POINT('Ctrl Pts',(83.4129472351165,-2.68048979719727,-2.58448281512371));
#16224=CARTESIAN_POINT('Ctrl Pts',(83.4189166499203,-2.6042955312153,-2.66036362449628));
#16225=CARTESIAN_POINT('Ctrl Pts',(83.4206730949348,-2.58135022513618,-2.68263321825345));
#16226=CARTESIAN_POINT('Ctrl Pts',(83.4237525950993,-2.5401170454266,-2.72163315304266));
#16227=CARTESIAN_POINT('Ctrl Pts',(83.4250837025986,-2.52194505370165,-2.73848038752581));
#16228=CARTESIAN_POINT('Ctrl Pts',(83.428133800469,-2.47949951325509,-2.77705069903226));
#16229=CARTESIAN_POINT('Ctrl Pts',(83.4298435096785,-2.45510713390138,-2.79863851276391));
#16230=CARTESIAN_POINT('Ctrl Pts',(83.4353841900916,-2.37423569819015,-2.86834041006189));
#16231=CARTESIAN_POINT('Ctrl Pts',(83.4391332259844,-2.31659896398363,-2.91508873796779));
#16232=CARTESIAN_POINT('Ctrl Pts',(83.4562313316096,-2.04283030676886,-3.12388683190406));
#16233=CARTESIAN_POINT('Ctrl Pts',(83.4687957904166,-1.81086280537036,-3.26383482825989));
#16234=CARTESIAN_POINT('Ctrl Pts',(83.4865013276209,-1.48078382492111,-3.4168588080493));
#16235=CARTESIAN_POINT('Ctrl Pts',(83.4911173468721,-1.39433277550477,-3.45303918718552));
#16236=CARTESIAN_POINT('Ctrl Pts',(83.4996044202193,-1.23619370674814,-3.51231378902122));
#16237=CARTESIAN_POINT('Ctrl Pts',(83.503440559873,-1.16499473470343,-3.53656745324965));
#16238=CARTESIAN_POINT('Ctrl Pts',(83.5097692295129,-1.04847164302234,-3.57235995571267));
#16239=CARTESIAN_POINT('Ctrl Pts',(83.5122193145197,-1.00357769368316,-3.58523081486505));
#16240=CARTESIAN_POINT('Ctrl Pts',(83.5170448962557,-0.915669737136947,
-3.60865307376034));
#16241=CARTESIAN_POINT('Ctrl Pts',(83.5194172781105,-0.872686049542964,
-3.61928817672618));
#16242=CARTESIAN_POINT('Ctrl Pts',(83.5252766768713,-0.76715499209866,-3.64340965513409));
#16243=CARTESIAN_POINT('Ctrl Pts',(83.5287890688095,-0.704431593327425,
-3.65605472398968));
#16244=CARTESIAN_POINT('Ctrl Pts',(83.5479355589096,-0.365508791770839,
-3.7153364127369));
#16245=CARTESIAN_POINT('Ctrl Pts',(83.5644682736973,-0.0850695691510357,
-3.73229717196538));
#16246=CARTESIAN_POINT('Ctrl Pts',(83.5901494371418,0.349343444480504,-3.70956166195331));
#16247=CARTESIAN_POINT('Ctrl Pts',(83.599251969939,0.50347247068095,-3.69180312697101));
#16248=CARTESIAN_POINT('Ctrl Pts',(83.6105841792651,0.701018548347868,-3.65643640446163));
#16249=CARTESIAN_POINT('Ctrl Pts',(83.6131317785146,0.745833250036449,-3.64755909004184));
#16250=CARTESIAN_POINT('Ctrl Pts',(83.6171034157223,0.816556591822837,-3.63219152268993));
#16251=CARTESIAN_POINT('Ctrl Pts',(83.6185541069433,0.842577328332253,-3.62624371398824));
#16252=CARTESIAN_POINT('Ctrl Pts',(83.6214284907893,0.894570768669446,-3.61376918284361));
#16253=CARTESIAN_POINT('Ctrl Pts',(83.6228520689543,0.920541386241129,-3.60724107993627));
#16254=CARTESIAN_POINT('Ctrl Pts',(83.626660835685,0.990528164418255,-3.58884376802237));
#16255=CARTESIAN_POINT('Ctrl Pts',(83.6290188571499,1.03440154186965,-3.57644508353148));
#16256=CARTESIAN_POINT('Ctrl Pts',(83.6439924781601,1.31539049994864,-3.49143355508272));
#16257=CARTESIAN_POINT('Ctrl Pts',(83.6556675390205,1.54499682541416,-3.39608140268703));
#16258=CARTESIAN_POINT('Ctrl Pts',(83.6762584420214,1.92246193854061,-3.19305734416994));
#16259=CARTESIAN_POINT('Ctrl Pts',(83.6850280132631,2.07504963653927,-3.09606799524797));
#16260=CARTESIAN_POINT('Ctrl Pts',(83.6975610776047,2.27376479873965,-2.94844856096181));
#16261=CARTESIAN_POINT('Ctrl Pts',(83.7009996631463,2.32645023892897,-2.90705759712991));
#16262=CARTESIAN_POINT('Ctrl Pts',(83.7068637641646,2.41298631487513,-2.83521316950821));
#16263=CARTESIAN_POINT('Ctrl Pts',(83.7092596483056,2.44744763878988,-2.80551893421772));
#16264=CARTESIAN_POINT('Ctrl Pts',(83.7138682796151,2.5119881525956,-2.74781215427669));
#16265=CARTESIAN_POINT('Ctrl Pts',(83.7160760309642,2.54216457518938,-2.71991823518722));
#16266=CARTESIAN_POINT('Ctrl Pts',(83.721987389539,2.62097551097681,-2.64461104187058));
#16267=CARTESIAN_POINT('Ctrl Pts',(83.7257256587852,2.66878319044914,-2.5963581547807));
#16268=CARTESIAN_POINT('Ctrl Pts',(83.7391975189689,2.83389782740182,-2.42032487271339));
#16269=CARTESIAN_POINT('Ctrl Pts',(83.7492167701334,2.94355601864174,-2.28569826721965));
#16270=CARTESIAN_POINT('Ctrl Pts',(83.7683380940237,3.1311565748759,-2.0193895395188));
#16271=CARTESIAN_POINT('Ctrl Pts',(83.7773825708992,3.21116203266535,-1.88958030309448));
#16272=CARTESIAN_POINT('Ctrl Pts',(83.7909849898624,3.32075020708103,-1.68460674672849));
#16273=CARTESIAN_POINT('Ctrl Pts',(83.7956313562862,3.35622403414705,-1.61277499397278));
#16274=CARTESIAN_POINT('Ctrl Pts',(83.8034261896783,3.41282162792539,-1.48819853785444));
#16275=CARTESIAN_POINT('Ctrl Pts',(83.8066151922318,3.43510619660879,-1.43601268065878));
#16276=CARTESIAN_POINT('Ctrl Pts',(83.8113432052663,3.46696084763822,-1.35642551886147));
#16277=CARTESIAN_POINT('Ctrl Pts',(83.8129261062509,3.47741716679819,-1.3293899585882));
#16278=CARTESIAN_POINT('Ctrl Pts',(83.815852574161,3.49637952445641,-1.27860623382985));
#16279=CARTESIAN_POINT('Ctrl Pts',(83.8171999813375,3.50496162937362,-1.25488950590697));
#16280=CARTESIAN_POINT('Ctrl Pts',(83.8205702077459,3.52602790945583,-1.19477010012411));
#16281=CARTESIAN_POINT('Ctrl Pts',(83.8225757723952,3.53819017308572,-1.15825685061596));
#16282=CARTESIAN_POINT('Ctrl Pts',(83.8314316637413,3.59003589499568,-0.994162997081114));
#16283=CARTESIAN_POINT('Ctrl Pts',(83.8379996857618,3.62340319225326,-0.86468069151639));
#16284=CARTESIAN_POINT('Ctrl Pts',(83.8548324462676,3.69193750290241,-0.52375039050757));
#16285=CARTESIAN_POINT('Ctrl Pts',(83.8649279586079,3.71594660558186,-0.310578219390088));
#16286=CARTESIAN_POINT('Ctrl Pts',(83.8796097384085,3.72372783165573,-0.0105687999832971));
#16287=CARTESIAN_POINT('Ctrl Pts',(83.8838691542674,3.72297856222137,0.0754333607792057));
#16288=CARTESIAN_POINT('Ctrl Pts',(83.8917805181,3.71618339616644,0.232087674670751));
#16289=CARTESIAN_POINT('Ctrl Pts',(83.8954053909491,3.71109564712829,0.302740841039616));
#16290=CARTESIAN_POINT('Ctrl Pts',(83.9014872494626,3.69937842238453,0.419032843454376));
#16291=CARTESIAN_POINT('Ctrl Pts',(83.9039088694483,3.69391074271478,0.464771357455509));
#16292=CARTESIAN_POINT('Ctrl Pts',(83.9087830496748,3.68133580642662,0.555625010578794));
#16293=CARTESIAN_POINT('Ctrl Pts',(83.9112347362656,3.6742442268481,0.600734205186967));
#16294=CARTESIAN_POINT('Ctrl Pts',(83.9174315923414,3.65443332525176,0.713221696609458));
#16295=CARTESIAN_POINT('Ctrl Pts',(83.9212077158701,3.64067926602818,0.780398466693295));
#16296=CARTESIAN_POINT('Ctrl Pts',(83.9356978252883,3.58165226936026,1.0329823251376));
#16297=CARTESIAN_POINT('Ctrl Pts',(83.9467707403151,3.5240059185411,1.21517639209199));
#16298=CARTESIAN_POINT('Ctrl Pts',(83.9679619862629,3.38942279659358,1.54895902919156));
#16299=CARTESIAN_POINT('Ctrl Pts',(83.9780162803526,3.31557685485957,1.70129732655008));
#16300=CARTESIAN_POINT('Ctrl Pts',(83.9914350912164,3.20079623001511,1.90200653607067));
#16301=CARTESIAN_POINT('Ctrl Pts',(83.9950041241817,3.16861639365688,1.95514607327778));
#16302=CARTESIAN_POINT('Ctrl Pts',(84.0011963757302,3.10956695795086,2.0473657594154));
#16303=CARTESIAN_POINT('Ctrl Pts',(84.0038426353865,3.08325237539411,2.0867842275118));
#16304=CARTESIAN_POINT('Ctrl Pts',(84.0079344242075,3.04071361213057,2.14794390756076));
#16305=CARTESIAN_POINT('Ctrl Pts',(84.009408934715,3.02499298892332,2.17002760526528));
#16306=CARTESIAN_POINT('Ctrl Pts',(84.0122906618612,2.99345399735384,2.21332345825535));
#16307=CARTESIAN_POINT('Ctrl Pts',(84.0136984279709,2.97764804758882,2.23454239822952));
#16308=CARTESIAN_POINT('Ctrl Pts',(84.017418342554,2.93486379641107,2.29071859921863));
#16309=CARTESIAN_POINT('Ctrl Pts',(84.0197053783879,2.90748675249781,2.32536842457618));
#16310=CARTESIAN_POINT('Ctrl Pts',(84.03259065013,2.74762096130101,2.52046423837457));
#16311=CARTESIAN_POINT('Ctrl Pts',(84.0425190135211,2.60247016200988,2.67007972286238));
#16312=CARTESIAN_POINT('Ctrl Pts',(84.0624031484007,2.28953368249273,2.94274220337305));
#16313=CARTESIAN_POINT('Ctrl Pts',(84.072331372375,2.1224436072201,3.06543991445343));
#16314=CARTESIAN_POINT('Ctrl Pts',(84.0864978851887,1.88231055164521,3.21268770257991));
#16315=CARTESIAN_POINT('Ctrl Pts',(84.0903134071336,1.81742641055444,3.24983316467351));
#16316=CARTESIAN_POINT('Ctrl Pts',(84.0966248541689,1.71020517253938,3.3070005657496));
#16317=CARTESIAN_POINT('Ctrl Pts',(84.0990793757297,1.66853007633547,3.32822198808082));
#16318=CARTESIAN_POINT('Ctrl Pts',(84.1039265587214,1.58636333652785,3.36813103886614));
#16319=CARTESIAN_POINT('Ctrl Pts',(84.1063163702875,1.54591376819017,3.38688732037933));
#16320=CARTESIAN_POINT('Ctrl Pts',(84.1122457380088,1.44576455455904,3.43115818723231));
#16321=CARTESIAN_POINT('Ctrl Pts',(84.1158116609776,1.38571725484166,3.45584557431743));
#16322=CARTESIAN_POINT('Ctrl Pts',(84.1346499696334,1.06956370073763,3.57626171697957));
#16323=CARTESIAN_POINT('Ctrl Pts',(84.1507648386761,0.804157548623636,3.64512084960632));
#16324=CARTESIAN_POINT('Ctrl Pts',(84.1762430953166,0.376943384656355,3.7070007311358));
#16325=CARTESIAN_POINT('Ctrl Pts',(84.1855479519405,0.218934516246659,3.71967940236616));
#16326=CARTESIAN_POINT('Ctrl Pts',(84.1970974593835,0.0144622026793799,
3.72300775562695));
#16327=CARTESIAN_POINT('Ctrl Pts',(84.1996708459668,-0.0316776945410093,
3.72290112718942));
#16328=CARTESIAN_POINT('Ctrl Pts',(84.2036770923633,-0.104657644209761,
3.72137550988149));
#16329=CARTESIAN_POINT('Ctrl Pts',(84.2051370643525,-0.131503616993609,
3.72052359140501));
#16330=CARTESIAN_POINT('Ctrl Pts',(84.2080174526266,-0.185030306576398,
3.71824489174586));
#16331=CARTESIAN_POINT('Ctrl Pts',(84.209437928948,-0.211709548058561,3.71682128132288));
#16332=CARTESIAN_POINT('Ctrl Pts',(84.2132328593006,-0.283654820992114,
3.71220507110036));
#16333=CARTESIAN_POINT('Ctrl Pts',(84.2155804119649,-0.328882759828231,
3.7084717908243));
#16334=CARTESIAN_POINT('Ctrl Pts',(84.2306036367792,-0.621877745031476,
3.678884215306));
#16335=CARTESIAN_POINT('Ctrl Pts',(84.2423267203417,-0.86660830598496,3.62904051580633));
#16336=CARTESIAN_POINT('Ctrl Pts',(84.2617401583419,-1.25251078999618,3.50914410478832));
#16337=CARTESIAN_POINT('Ctrl Pts',(84.2692526983368,-1.3974573896755,3.45398091650242));
#16338=CARTESIAN_POINT('Ctrl Pts',(84.2809982225684,-1.61085106516936,3.35713160301902));
#16339=CARTESIAN_POINT('Ctrl Pts',(84.2850400742585,-1.68209134678154,3.32200863327877));
#16340=CARTESIAN_POINT('Ctrl Pts',(84.2916274983343,-1.79418963292394,3.26221109529338));
#16341=CARTESIAN_POINT('Ctrl Pts',(84.2941241706537,-1.83579234461218,3.2389819182649));
#16342=CARTESIAN_POINT('Ctrl Pts',(84.299016557877,-1.91552886629479,3.19243069134184));
#16343=CARTESIAN_POINT('Ctrl Pts',(84.3014085125211,-1.95371112459508,3.16920765592025));
#16344=CARTESIAN_POINT('Ctrl Pts',(84.3072071267281,-2.04430897257305,3.11184516564172));
#16345=CARTESIAN_POINT('Ctrl Pts',(84.3106364169776,-2.0962989975848,3.07706181085706));
#16346=CARTESIAN_POINT('Ctrl Pts',(84.3255913422868,-2.3161779157726,2.9217947892804));
#16347=CARTESIAN_POINT('Ctrl Pts',(84.3375608740159,-2.47462004730783,2.78884999307511));
#16348=CARTESIAN_POINT('Ctrl Pts',(84.3497092113127,-2.62112002533992,2.64359553927261));
#16349=CARTESIAN_POINT('Origin',(80.1322559480305,0.,0.));
#16350=CARTESIAN_POINT('',(85.8498933978769,-2.62112000707361,2.64359555738363));
#16351=CARTESIAN_POINT('',(85.6021262427416,-2.62112000930789,2.64359555516834));
#16352=CARTESIAN_POINT('',(80.1322559480305,-2.62112000711956,2.64359555733806));
#16353=CARTESIAN_POINT('',(84.7537451115017,-3.72274958225736,-0.00176360502600202));
#16354=CARTESIAN_POINT('Ctrl Pts',(85.8498933978769,-2.62112000707361,2.64359555738363));
#16355=CARTESIAN_POINT('Ctrl Pts',(85.849690671865,-2.6184134442255,2.64627910934065));
#16356=CARTESIAN_POINT('Ctrl Pts',(85.8494877682365,-2.6157027508985,2.64895851394654));
#16357=CARTESIAN_POINT('Ctrl Pts',(85.8467827579202,-2.57954191884002,2.6845923255638));
#16358=CARTESIAN_POINT('Ctrl Pts',(85.8442541779368,-2.54547641486122,2.7169140613065));
#16359=CARTESIAN_POINT('Ctrl Pts',(85.8375783888193,-2.45491206316508,2.79964394224953));
#16360=CARTESIAN_POINT('Ctrl Pts',(85.833389512113,-2.39747278233872,2.84898623874646));
#16361=CARTESIAN_POINT('Ctrl Pts',(85.8193038106923,-2.20236979897572,3.00650596879077));
#16362=CARTESIAN_POINT('Ctrl Pts',(85.8091355210378,-2.05859394793133,3.10671713627308));
#16363=CARTESIAN_POINT('Ctrl Pts',(85.7844201176763,-1.69807556203329,3.32195157666296));
#16364=CARTESIAN_POINT('Ctrl Pts',(85.7697852079376,-1.4759574290867,3.42642423730708));
#16365=CARTESIAN_POINT('Ctrl Pts',(85.7537493346471,-1.20683816778594,3.52194047344496));
#16366=CARTESIAN_POINT('Ctrl Pts',(85.7514911153441,-1.16827171348717,3.53492072508049));
#16367=CARTESIAN_POINT('Ctrl Pts',(85.7479931769934,-1.1073266952543,3.55432646112222));
#16368=CARTESIAN_POINT('Ctrl Pts',(85.7467314252218,-1.0850882112766,3.5611785482578));
#16369=CARTESIAN_POINT('Ctrl Pts',(85.7440235336394,-1.03676569334935,3.57557290535865));
#16370=CARTESIAN_POINT('Ctrl Pts',(85.7425816923323,-1.01066044131974,3.5830392497816));
#16371=CARTESIAN_POINT('Ctrl Pts',(85.7386547552395,-0.938620784840327,
3.60279326329947));
#16372=CARTESIAN_POINT('Ctrl Pts',(85.7361999030544,-0.892527813711963,
3.6144878986108));
#16373=CARTESIAN_POINT('Ctrl Pts',(85.7306046011122,-0.785460212401721,
3.63947975819947));
#16374=CARTESIAN_POINT('Ctrl Pts',(85.7274902187997,-0.724349407330987,
3.65213351651395));
#16375=CARTESIAN_POINT('Ctrl Pts',(85.7160022790089,-0.494949250037407,
3.69364865955921));
#16376=CARTESIAN_POINT('Ctrl Pts',(85.7078909325865,-0.325052530382849,
3.71246019291951));
#16377=CARTESIAN_POINT('Ctrl Pts',(85.6906654259996,0.0336435509885337,
3.72735554171201));
#16378=CARTESIAN_POINT('Ctrl Pts',(85.6815524370027,0.222057317023121,3.72088623031167));
#16379=CARTESIAN_POINT('Ctrl Pts',(85.6685746735745,0.477207648111928,3.69267210153699));
#16380=CARTESIAN_POINT('Ctrl Pts',(85.6650649689563,0.545029842721874,3.68327247522413));
#16381=CARTESIAN_POINT('Ctrl Pts',(85.6591208615526,0.6575800274808,3.66449724096061));
#16382=CARTESIAN_POINT('Ctrl Pts',(85.656718348156,0.702464850401875,3.65615842317771));
#16383=CARTESIAN_POINT('Ctrl Pts',(85.6518382467234,0.792342665615207,3.6377445746562));
#16384=CARTESIAN_POINT('Ctrl Pts',(85.6493605835827,0.83732439850672,3.62765490176853));
#16385=CARTESIAN_POINT('Ctrl Pts',(85.6430018368033,0.951063617474324,3.59991438627524));
#16386=CARTESIAN_POINT('Ctrl Pts',(85.63908630388,1.01952279049039,3.58112802790292));
#16387=CARTESIAN_POINT('Ctrl Pts',(85.6302875271805,1.16987179069909,3.53520912508429));
#16388=CARTESIAN_POINT('Ctrl Pts',(85.6253796023952,1.25143887867322,3.50716450216352));
#16389=CARTESIAN_POINT('Ctrl Pts',(85.6079786913726,1.53320161432178,3.39920670606868));
#16390=CARTESIAN_POINT('Ctrl Pts',(85.5951510989502,1.72736505329527,3.30477133006903));
#16391=CARTESIAN_POINT('Ctrl Pts',(85.5747142866102,2.02577702016933,3.12611610337083));
#16392=CARTESIAN_POINT('Ctrl Pts',(85.5670243972746,2.13560545026952,3.05214170424462));
#16393=CARTESIAN_POINT('Ctrl Pts',(85.5574720328277,2.27182319314675,2.94943237272094));
#16394=CARTESIAN_POINT('Ctrl Pts',(85.5553535574472,2.30202223251655,2.9259230696851));
#16395=CARTESIAN_POINT('Ctrl Pts',(85.5518912440141,2.35146525431007,2.88619327484354));
#16396=CARTESIAN_POINT('Ctrl Pts',(85.5505308828231,2.37091645121678,2.87023618807598));
#16397=CARTESIAN_POINT('Ctrl Pts',(85.5476361342394,2.4123897687681,2.83550356354633));
#16398=CARTESIAN_POINT('Ctrl Pts',(85.5461059159884,2.43435717266661,2.81666648997742));
#16399=CARTESIAN_POINT('Ctrl Pts',(85.5416194178792,2.49878774444922,2.76010029706633));
#16400=CARTESIAN_POINT('Ctrl Pts',(85.5387092671786,2.54061097516456,2.72165213478155));
#16401=CARTESIAN_POINT('Ctrl Pts',(85.5317968229488,2.63937172582106,2.62659990025905));
#16402=CARTESIAN_POINT('Ctrl Pts',(85.5278415292646,2.69539094125685,2.56908134265731));
#16403=CARTESIAN_POINT('Ctrl Pts',(85.5165010950126,2.85244590106617,2.39702580300335));
#16404=CARTESIAN_POINT('Ctrl Pts',(85.50924685486,2.94834958500859,2.27802919945283));
#16405=CARTESIAN_POINT('Ctrl Pts',(85.4935449089584,3.13734262298577,2.01152504874999));
#16406=CARTESIAN_POINT('Ctrl Pts',(85.4850867484135,3.22792573528098,1.86269716150979));
#16407=CARTESIAN_POINT('Ctrl Pts',(85.4728497410405,3.33893488953635,1.64772475897147));
#16408=CARTESIAN_POINT('Ctrl Pts',(85.4693655046101,3.36844673677804,1.58652101842006));
#16409=CARTESIAN_POINT('Ctrl Pts',(85.4636886265646,3.41306288591806,1.48712861096727));
#16410=CARTESIAN_POINT('Ctrl Pts',(85.4615317343766,3.42923932167846,1.44943688014956));
#16411=CARTESIAN_POINT('Ctrl Pts',(85.4569480635662,3.46197230741317,1.36955071887326));
#16412=CARTESIAN_POINT('Ctrl Pts',(85.4545171095525,3.4783875643555,1.32730597020498));
#16413=CARTESIAN_POINT('Ctrl Pts',(85.4484547514622,3.51699110628418,1.22232104980251));
#16414=CARTESIAN_POINT('Ctrl Pts',(85.444795266573,3.538275535791,1.15926729498409));
#16415=CARTESIAN_POINT('Ctrl Pts',(85.4311615839286,3.61023463082996,0.925603878823073));
#16416=CARTESIAN_POINT('Ctrl Pts',(85.4208784736446,3.65034344467164,0.752009042050682));
#16417=CARTESIAN_POINT('Ctrl Pts',(85.3955882918672,3.71698579221673,0.326652004638766));
#16418=CARTESIAN_POINT('Ctrl Pts',(85.3804520176507,3.73058373419855,0.0737393952907888));
#16419=CARTESIAN_POINT('Ctrl Pts',(85.3636757419601,3.71631345849157,-0.223359226114893));
#16420=CARTESIAN_POINT('Ctrl Pts',(85.36117938238,3.71335598082205,-0.268072326452417));
#16421=CARTESIAN_POINT('Ctrl Pts',(85.3572634888432,3.70735760461216,-0.339226442226781));
#16422=CARTESIAN_POINT('Ctrl Pts',(85.3558187653444,3.70483928268253,-0.365706135442116));
#16423=CARTESIAN_POINT('Ctrl Pts',(85.3529395161141,3.69919392747321,-0.418999304245632));
#16424=CARTESIAN_POINT('Ctrl Pts',(85.3515054731768,3.69605864120948,-0.445810204152075));
#16425=CARTESIAN_POINT('Ctrl Pts',(85.3476264503708,3.68669599884262,-0.518966908123563));
#16426=CARTESIAN_POINT('Ctrl Pts',(85.3452104894457,3.67988647037834,-0.565234446341687));
#16427=CARTESIAN_POINT('Ctrl Pts',(85.3344763028182,3.64527779241602,-0.773114466746253));
#16428=CARTESIAN_POINT('Ctrl Pts',(85.3265494915856,3.60768891066312,-0.932922966576545));
#16429=CARTESIAN_POINT('Ctrl Pts',(85.306004472804,3.48241018388323,-1.34215037544668));
#16430=CARTESIAN_POINT('Ctrl Pts',(85.2934810245839,3.37851977141229,-1.58560494221275));
#16431=CARTESIAN_POINT('Ctrl Pts',(85.2767595163137,3.21750684931743,-1.8737364836297));
#16432=CARTESIAN_POINT('Ctrl Pts',(85.2733641118959,3.18372448134068,-1.93057931628217));
#16433=CARTESIAN_POINT('Ctrl Pts',(85.2675795871691,3.12454326829097,-2.02437737777324));
#16434=CARTESIAN_POINT('Ctrl Pts',(85.2652194988286,3.09995760553115,-2.06182856209323));
#16435=CARTESIAN_POINT('Ctrl Pts',(85.2603592027751,3.04848611462761,-2.13723240205437));
#16436=CARTESIAN_POINT('Ctrl Pts',(85.257857514359,3.02155299329874,-2.17514302465089));
#16437=CARTESIAN_POINT('Ctrl Pts',(85.2513488598448,2.95040283633244,-2.27142055647856));
#16438=CARTESIAN_POINT('Ctrl Pts',(85.247304087132,2.90516269536378,-2.32900342355141));
#16439=CARTESIAN_POINT('Ctrl Pts',(85.2381486347237,2.80054002858953,-2.45437522820134));
#16440=CARTESIAN_POINT('Ctrl Pts',(85.233009787767,2.74033565318834,-2.52141648531876));
#16441=CARTESIAN_POINT('Ctrl Pts',(85.2138900374879,2.51055586160951,-2.75933095029729));
#16442=CARTESIAN_POINT('Ctrl Pts',(85.1994926721621,2.32695572552251,-2.91582994796519));
#16443=CARTESIAN_POINT('Ctrl Pts',(85.1794133401151,2.04470101149989,-3.11267855988058));
#16444=CARTESIAN_POINT('Ctrl Pts',(85.1734583055322,1.95741008072819,-3.16829903621415));
#16445=CARTESIAN_POINT('Ctrl Pts',(85.1656614014065,1.83662806856286,-3.238359571677));
#16446=CARTESIAN_POINT('Ctrl Pts',(85.1636642298542,1.80508217280523,-3.25604882050573));
#16447=CARTESIAN_POINT('Ctrl Pts',(85.1603248978248,1.75119397463262,-3.28524250485353));
#16448=CARTESIAN_POINT('Ctrl Pts',(85.1589692673526,1.72898460721741,-3.29698513832612));
#16449=CARTESIAN_POINT('Ctrl Pts',(85.1560187909301,1.6798857445708,-3.32231226848747));
#16450=CARTESIAN_POINT('Ctrl Pts',(85.1544295912095,1.65294767942693,-3.3357966079129));
#16451=CARTESIAN_POINT('Ctrl Pts',(85.1495438452933,1.56873275593393,-3.37668122870755));
#16452=CARTESIAN_POINT('Ctrl Pts',(85.1463066382227,1.51091439842671,-3.40294535709103));
#16453=CARTESIAN_POINT('Ctrl Pts',(85.1383752689073,1.3652789044957,-3.46465643146747));
#16454=CARTESIAN_POINT('Ctrl Pts',(85.1337487411319,1.27672671808013,-3.49825687718033));
#16455=CARTESIAN_POINT('Ctrl Pts',(85.1141347012584,0.892244002792272,-3.62759872028588));
#16456=CARTESIAN_POINT('Ctrl Pts',(85.0995838599321,0.586259359639179,-3.68942663553642));
#16457=CARTESIAN_POINT('Ctrl Pts',(85.0805513678091,0.212363743369056,-3.71723823530693));
#16458=CARTESIAN_POINT('Ctrl Pts',(85.0772610466554,0.148470781483462,-3.72033792503272));
#16459=CARTESIAN_POINT('Ctrl Pts',(85.0716002164644,0.0400926945410302,
-3.72279948451585));
#16460=CARTESIAN_POINT('Ctrl Pts',(85.0692557557627,-0.00435970776291281,
-3.72301278485109));
#16461=CARTESIAN_POINT('Ctrl Pts',(85.0643789373947,-0.0958629766291269,
-3.72181310301018));
#16462=CARTESIAN_POINT('Ctrl Pts',(85.0618440808799,-0.142904408503924,
-3.72030382385572));
#16463=CARTESIAN_POINT('Ctrl Pts',(85.0551293303995,-0.266093901446509,
-3.71401154633122));
#16464=CARTESIAN_POINT('Ctrl Pts',(85.0509068507374,-0.342142874098028,
-3.70777896439628));
#16465=CARTESIAN_POINT('Ctrl Pts',(85.0362181452921,-0.601868186238297,
-3.67843478434));
#16466=CARTESIAN_POINT('Ctrl Pts',(85.0254414107457,-0.783969729701323,
-3.64396859276095));
#16467=CARTESIAN_POINT('Ctrl Pts',(85.0009552627431,-1.18532731820022,-3.53651868552044));
#16468=CARTESIAN_POINT('Ctrl Pts',(84.9872180388399,-1.40191405716723,-3.45638720978235));
#16469=CARTESIAN_POINT('Ctrl Pts',(84.9718707338294,-1.64789446364138,-3.33842850674785));
#16470=CARTESIAN_POINT('Ctrl Pts',(84.9695164666197,-1.68576682161008,-3.31946555624318));
#16471=CARTESIAN_POINT('Ctrl Pts',(84.9659081034696,-1.74418278175617,-3.2889585801291));
#16472=CARTESIAN_POINT('Ctrl Pts',(84.9646297084749,-1.76495336420293,-3.27785933186331));
#16473=CARTESIAN_POINT('Ctrl Pts',(84.961927736748,-1.80905081171537,-3.25375412549343));
#16474=CARTESIAN_POINT('Ctrl Pts',(84.960507774711,-1.83234598235991,-3.24069267713044));
#16475=CARTESIAN_POINT('Ctrl Pts',(84.9567150874877,-1.89480801702728,-3.20478174982224));
#16476=CARTESIAN_POINT('Ctrl Pts',(84.9543692210441,-1.9337023210387,-3.18146493993844));
#16477=CARTESIAN_POINT('Ctrl Pts',(84.9443354643363,-2.10051263966192,-3.07727394809547));
#16478=CARTESIAN_POINT('Ctrl Pts',(84.9369827810126,-2.22386541700076,-2.98934740188423));
#16479=CARTESIAN_POINT('Ctrl Pts',(84.9159627626948,-2.56360247213679,-2.71448092137758));
#16480=CARTESIAN_POINT('Ctrl Pts',(84.9024776027734,-2.76424147811763,-2.50986546867904));
#16481=CARTESIAN_POINT('Ctrl Pts',(84.8847550471818,-2.97832064635667,-2.23438445737353));
#16482=CARTESIAN_POINT('Ctrl Pts',(84.8814995092742,-3.01584937030715,-2.18346508142242));
#16483=CARTESIAN_POINT('Ctrl Pts',(84.8758793316965,-3.07745041164041,-2.09526432294667));
#16484=CARTESIAN_POINT('Ctrl Pts',(84.8735397712441,-3.10218702154537,-2.05846279565114));
#16485=CARTESIAN_POINT('Ctrl Pts',(84.8686558052075,-3.15192662118896,-1.98152995368773));
#16486=CARTESIAN_POINT('Ctrl Pts',(84.8661085388942,-3.17683413205588,-1.94134669859161));
#16487=CARTESIAN_POINT('Ctrl Pts',(84.8593165320083,-3.24050823784929,-1.83411320327146));
#16488=CARTESIAN_POINT('Ctrl Pts',(84.8550273615134,-3.2779579375688,-1.76631125667132));
#16489=CARTESIAN_POINT('Ctrl Pts',(84.8412594319495,-3.38956998045064,-1.548447751507));
#16490=CARTESIAN_POINT('Ctrl Pts',(84.831543517956,-3.45573829440158,-1.39453892485221));
#16491=CARTESIAN_POINT('Ctrl Pts',(84.8202647296711,-3.51942678638267,-1.21371224090924));
#16492=CARTESIAN_POINT('Ctrl Pts',(84.818827801575,-3.52730213564476,-1.19063090082885));
#16493=CARTESIAN_POINT('Ctrl Pts',(84.8045260992239,-3.60334936767769,-0.960370371252661));
#16494=CARTESIAN_POINT('Ctrl Pts',(84.791550227207,-3.65341923644053,-0.747646651339363));
#16495=CARTESIAN_POINT('Ctrl Pts',(84.7767654333701,-3.69088600924998,-0.488036032550343));
#16496=CARTESIAN_POINT('Ctrl Pts',(84.7743057493962,-3.69641713113331,-0.444206515957367));
#16497=CARTESIAN_POINT('Ctrl Pts',(84.7704330357799,-3.70401337983993,-0.373969471396635));
#16498=CARTESIAN_POINT('Ctrl Pts',(84.7689957101955,-3.70657900291763,-0.34762118329231));
#16499=CARTESIAN_POINT('Ctrl Pts',(84.7663402017868,-3.71084565512058,-0.298361757564472));
#16500=CARTESIAN_POINT('Ctrl Pts',(84.7651181604813,-3.71261605647989,-0.275458319804983));
#16501=CARTESIAN_POINT('Ctrl Pts',(84.7620086973118,-3.71661573803118,-0.216633771789246));
#16502=CARTESIAN_POINT('Ctrl Pts',(84.7601367848935,-3.71853638012616,-0.18069339852061));
#16503=CARTESIAN_POINT('Ctrl Pts',(84.755838637514,-3.72178703021132,-0.0971430511158404));
#16504=CARTESIAN_POINT('Ctrl Pts',(84.7534291834744,-3.7227252296709,-0.0495238594225499));
#16505=CARTESIAN_POINT('Ctrl Pts',(84.7510485996216,-3.72274951596391,-0.0018983915450042));
#16506=CARTESIAN_POINT('Ctrl Pts',(84.5967274725783,-2.62112000711956,2.64359555733807));
#16507=CARTESIAN_POINT('Ctrl Pts',(84.6026171986451,-2.69922371257001,2.56615588075135));
#16508=CARTESIAN_POINT('Ctrl Pts',(84.6085069247118,-2.77399981426397,2.48514542701443));
#16509=CARTESIAN_POINT('Ctrl Pts',(84.6143966507786,-2.8451029650521,2.40088664471102));
#16510=CARTESIAN_POINT('Ctrl Pts',(84.6202805304275,-2.91613553552328,2.31671150162044));
#16511=CARTESIAN_POINT('Ctrl Pts',(84.6261644100763,-2.98350213256905,2.22929476853713));
#16512=CARTESIAN_POINT('Ctrl Pts',(84.6320482897252,-3.04689454055936,2.13899537662183));
#16513=CARTESIAN_POINT('Ctrl Pts',(84.6379289762132,-3.11025254571151,2.04874498987079));
#16514=CARTESIAN_POINT('Ctrl Pts',(84.6438096627011,-3.16964040204038,1.95561540157729));
#16515=CARTESIAN_POINT('Ctrl Pts',(84.6496903491891,-3.22479085590767,1.8599977145562));
#16516=CARTESIAN_POINT('Ctrl Pts',(84.6555693742753,-3.27992572876026,1.76440704128536));
#16517=CARTESIAN_POINT('Ctrl Pts',(84.6614483993615,-3.3308253651958,1.66633003653838));
#16518=CARTESIAN_POINT('Ctrl Pts',(84.6673274244476,-3.37726694254101,1.56618503418967));
#16519=CARTESIAN_POINT('Ctrl Pts',(84.6732063181649,-3.42370748213289,1.46604226961615));
#16520=CARTESIAN_POINT('Ctrl Pts',(84.6790852118822,-3.46568998202649,1.36383198771931));
#16521=CARTESIAN_POINT('Ctrl Pts',(84.6849641055995,-3.50303890758951,1.259994434279));
#16522=CARTESIAN_POINT('Ctrl Pts',(84.6908477122249,-3.54041777450897,1.15607363782295));
#16523=CARTESIAN_POINT('Ctrl Pts',(84.6967313188503,-3.57315550128109,1.05052336672847));
#16524=CARTESIAN_POINT('Ctrl Pts',(84.7026149254756,-3.60112584615127,0.943800933820955));
#16525=CARTESIAN_POINT('Ctrl Pts',(84.7085008428755,-3.62910717631744,0.837036585895238));
#16526=CARTESIAN_POINT('Ctrl Pts',(84.7143867602754,-3.65231730426597,0.729099577227213));
#16527=CARTESIAN_POINT('Ctrl Pts',(84.7202726776752,-3.67068113579185,0.620457542336191));
#16528=CARTESIAN_POINT('Ctrl Pts',(84.7261672436868,-3.68907195064722,0.511655871705734));
#16529=CARTESIAN_POINT('Ctrl Pts',(84.7320618096985,-3.70260218924548,0.402147529924563));
#16530=CARTESIAN_POINT('Ctrl Pts',(84.73795637571,-3.71124864543577,0.292405633070136));
#16531=CARTESIAN_POINT('Ctrl Pts',(84.7432192876406,-3.7189685585475,0.194423536152382));
#16532=CARTESIAN_POINT('Ctrl Pts',(84.7484821995711,-3.72279601755899,0.0962555076601766));
#16533=CARTESIAN_POINT('Ctrl Pts',(84.7537451115017,-3.72274958225736,-0.00176360502600202));
#16534=CARTESIAN_POINT('Ctrl Pts',(84.3497092113127,-2.62112002533992,2.64359553927261));
#16535=CARTESIAN_POINT('Ctrl Pts',(84.3546425218072,-2.68061210737739,2.58460925137001));
#16536=CARTESIAN_POINT('Ctrl Pts',(84.3596011602631,-2.73813507340312,2.52359289680976));
#16537=CARTESIAN_POINT('Ctrl Pts',(84.3709873311534,-2.86576174273039,2.37869753085833));
#16538=CARTESIAN_POINT('Ctrl Pts',(84.3773963270634,-2.93430300190607,2.29361290023421));
#16539=CARTESIAN_POINT('Ctrl Pts',(84.3876729138189,-3.04025380739108,2.14955135947495));
#16540=CARTESIAN_POINT('Ctrl Pts',(84.3916171678889,-3.079921981068,2.09231832310341));
#16541=CARTESIAN_POINT('Ctrl Pts',(84.3971995718364,-3.13497507960041,2.00792634534748));
#16542=CARTESIAN_POINT('Ctrl Pts',(84.3989069315164,-3.1516591772335,1.9816360710892));
#16543=CARTESIAN_POINT('Ctrl Pts',(84.401947187844,-3.18113105962466,1.93388126126274));
#16544=CARTESIAN_POINT('Ctrl Pts',(84.403286765783,-3.19403518993944,1.91249334613323));
#16545=CARTESIAN_POINT('Ctrl Pts',(84.4064525911418,-3.22432020005884,1.86113589718298));
#16546=CARTESIAN_POINT('Ctrl Pts',(84.4082669282372,-3.2414995419462,1.83105119208179));
#16547=CARTESIAN_POINT('Ctrl Pts',(84.4146894730729,-3.3015222850743,1.72244550386871));
#16548=CARTESIAN_POINT('Ctrl Pts',(84.4191753486541,-3.34195496938704,1.64262196725123));
#16549=CARTESIAN_POINT('Ctrl Pts',(84.4361098694402,-3.48615963720086,1.3305100808022));
#16550=CARTESIAN_POINT('Ctrl Pts',(84.4479914823629,-3.56890153561116,1.08927441714604));
#16551=CARTESIAN_POINT('Ctrl Pts',(84.4668897857842,-3.65653965255822,0.711592481441709));
#16552=CARTESIAN_POINT('Ctrl Pts',(84.473507464344,-3.67967662088619,0.58019128387289));
#16553=CARTESIAN_POINT('Ctrl Pts',(84.4831974327259,-3.70244347491494,0.392311637265982));
#16554=CARTESIAN_POINT('Ctrl Pts',(84.4860959566969,-3.70791962231769,0.336641886761319));
#16555=CARTESIAN_POINT('Ctrl Pts',(84.4913155253879,-3.71542002257566,0.237512876096766));
#16556=CARTESIAN_POINT('Ctrl Pts',(84.4936210795109,-3.71794066887489,0.194101216628514));
#16557=CARTESIAN_POINT('Ctrl Pts',(84.498661511634,-3.72174915842175,0.100069848188601));
#16558=CARTESIAN_POINT('Ctrl Pts',(84.5014041514759,-3.72276581131591,0.0494484318281852));
#16559=CARTESIAN_POINT('Ctrl Pts',(84.5094561643464,-3.72271936821563,-0.0975257749299699));
#16560=CARTESIAN_POINT('Ctrl Pts',(84.5148444201971,-3.71894850872693,-0.193831203364285));
#16561=CARTESIAN_POINT('Ctrl Pts',(84.5280396087446,-3.70089586081381,-0.424969055916771));
#16562=CARTESIAN_POINT('Ctrl Pts',(84.5359321790091,-3.6829774649357,-0.55937598081174));
#16563=CARTESIAN_POINT('Ctrl Pts',(84.5578033575243,-3.61382963707513,-0.924614276726773));
#16564=CARTESIAN_POINT('Ctrl Pts',(84.5719207963187,-3.54788959126416,-1.1520258440117));
#16565=CARTESIAN_POINT('Ctrl Pts',(84.5879553685414,-3.44339907249679,-1.4156663398813));
#16566=CARTESIAN_POINT('Ctrl Pts',(84.5905984927436,-3.42511900395839,-1.45933840121242));
#16567=CARTESIAN_POINT('Ctrl Pts',(84.5946871583552,-3.39506901312689,-1.52745170224194));
#16568=CARTESIAN_POINT('Ctrl Pts',(84.5961615701025,-3.38385700256842,-1.55213214073889));
#16569=CARTESIAN_POINT('Ctrl Pts',(84.5990449603415,-3.36115602275812,-1.60068721937661));
#16570=CARTESIAN_POINT('Ctrl Pts',(84.6004544532229,-3.34967987386434,-1.62456584571078));
#16571=CARTESIAN_POINT('Ctrl Pts',(84.6041824903521,-3.3183437910243,-1.68802332653556));
#16572=CARTESIAN_POINT('Ctrl Pts',(84.6064757621696,-3.29803040588654,-1.7273748962317));
#16573=CARTESIAN_POINT('Ctrl Pts',(84.6116274072054,-3.25017685600444,-1.81615482901501));
#16574=CARTESIAN_POINT('Ctrl Pts',(84.6144653321263,-3.22220205097662,-1.86533707402179));
#16575=CARTESIAN_POINT('Ctrl Pts',(84.624236301421,-3.1207866644609,-2.03453981501924));
#16576=CARTESIAN_POINT('Ctrl Pts',(84.6309798232979,-3.04167118982644,-2.15102335977938));
#16577=CARTESIAN_POINT('Ctrl Pts',(84.648701250769,-2.81686819763753,-2.4447147784816));
#16578=CARTESIAN_POINT('Ctrl Pts',(84.6596661181123,-2.66108963499289,-2.61342103503158));
#16579=CARTESIAN_POINT('Ctrl Pts',(84.6747278479668,-2.43958292500034,-2.81283707854977));
#16580=CARTESIAN_POINT('Ctrl Pts',(84.6782598319896,-2.38709498621008,-2.85751536462328));
#16581=CARTESIAN_POINT('Ctrl Pts',(84.6842305044487,-2.29776786785886,-2.92937220770402));
#16582=CARTESIAN_POINT('Ctrl Pts',(84.6866366374356,-2.26161251891279,-2.95737506564155));
#16583=CARTESIAN_POINT('Ctrl Pts',(84.6915151082924,-2.18806669136302,-3.01219989859036));
#16584=CARTESIAN_POINT('Ctrl Pts',(84.693987330951,-2.15067652219217,-3.03900877225089));
#16585=CARTESIAN_POINT('Ctrl Pts',(84.7003124425367,-2.05477241656622,-3.10511594194083));
#16586=CARTESIAN_POINT('Ctrl Pts',(84.7041990459056,-1.9956233393541,-3.14345690006567));
#16587=CARTESIAN_POINT('Ctrl Pts',(84.712918677061,-1.86248836521959,-3.22448363374186));
#16588=CARTESIAN_POINT('Ctrl Pts',(84.7177756466539,-1.78805082798849,-3.26634818049653));
#16589=CARTESIAN_POINT('Ctrl Pts',(84.7348299721388,-1.52531747284678,-3.40243888500404));
#16590=CARTESIAN_POINT('Ctrl Pts',(84.7473468256508,-1.33052279992698,-3.4832288539473));
#16591=CARTESIAN_POINT('Ctrl Pts',(84.76788386942,-0.997850851148307,-3.58920405298518));
#16592=CARTESIAN_POINT('Ctrl Pts',(84.7759570145586,-0.863481240740499,
-3.62387885383581));
#16593=CARTESIAN_POINT('Ctrl Pts',(84.7858809971974,-0.68971368566898,-3.65850319749194));
#16594=CARTESIAN_POINT('Ctrl Pts',(84.7880135066625,-0.6518297348069,-3.66544251646989));
#16595=CARTESIAN_POINT('Ctrl Pts',(84.7914917940829,-0.588994228358466,
-3.67594723925156));
#16596=CARTESIAN_POINT('Ctrl Pts',(84.7928544193103,-0.564102494804995,
-3.67984929239526));
#16597=CARTESIAN_POINT('Ctrl Pts',(84.7957460590942,-0.510644344919281,
-3.68767421882953));
#16598=CARTESIAN_POINT('Ctrl Pts',(84.7972710677173,-0.482068855933844,
-3.6915184562593));
#16599=CARTESIAN_POINT('Ctrl Pts',(84.8017233148346,-0.397639780640664,
-3.70187951412336));
#16600=CARTESIAN_POINT('Ctrl Pts',(84.8046054858955,-0.341678089832645,
-3.7074635570398));
#16601=CARTESIAN_POINT('Ctrl Pts',(84.8114337865579,-0.206743936676068,
-3.71784628455022));
#16602=CARTESIAN_POINT('Ctrl Pts',(84.8153344486984,-0.127702141772687,
-3.72139991209022));
#16603=CARTESIAN_POINT('Ctrl Pts',(84.8345807201097,0.267364908873462,-3.7265583250506));
#16604=CARTESIAN_POINT('Ctrl Pts',(84.849260887943,0.582562327217847,-3.69044016638166));
#16605=CARTESIAN_POINT('Ctrl Pts',(84.8689025965965,0.961687145052707,-3.59716061791241));
#16606=CARTESIAN_POINT('Ctrl Pts',(84.8727024635736,1.03340423358019,-3.57721699737138));
#16607=CARTESIAN_POINT('Ctrl Pts',(84.8789959196215,1.14909197302861,-3.54127635666802));
#16608=CARTESIAN_POINT('Ctrl Pts',(84.8814486566974,1.19344497172963,-3.52657616399787));
#16609=CARTESIAN_POINT('Ctrl Pts',(84.8863255408438,1.28011183520681,-3.49602943283517));
#16610=CARTESIAN_POINT('Ctrl Pts',(84.8887475227697,1.32243718193637,-3.48023961326192));
#16611=CARTESIAN_POINT('Ctrl Pts',(84.8947511138191,1.42554981714395,-3.43962002105868));
#16612=CARTESIAN_POINT('Ctrl Pts',(84.8983595747667,1.48598597784304,-3.41394538787247));
#16613=CARTESIAN_POINT('Ctrl Pts',(84.9145404220927,1.75016928798928,-3.29337016027291));
#16614=CARTESIAN_POINT('Ctrl Pts',(84.9276492091179,1.94573484863204,-3.18174053458709));
#16615=CARTESIAN_POINT('Ctrl Pts',(84.9532420129863,2.30141313122155,-2.93360502451104));
#16616=CARTESIAN_POINT('Ctrl Pts',(84.9656507130217,2.46244362557708,-2.79980746806889));
#16617=CARTESIAN_POINT('Ctrl Pts',(84.9799184722144,2.64285480987267,-2.62223831936189));
#16618=CARTESIAN_POINT('Ctrl Pts',(84.9823759499848,2.67375720602408,-2.59072153768956));
#16619=CARTESIAN_POINT('Ctrl Pts',(84.9862461200811,2.72228230590524,-2.53943832032324));
#16620=CARTESIAN_POINT('Ctrl Pts',(84.9876830526767,2.74026671316064,-2.52002110810626));
#16621=CARTESIAN_POINT('Ctrl Pts',(84.9905624032274,2.77627622563386,-2.48030135313373));
#16622=CARTESIAN_POINT('Ctrl Pts',(84.9920040440085,2.79428925589946,-2.45999026957238));
#16623=CARTESIAN_POINT('Ctrl Pts',(84.9959297417642,2.84322275496985,-2.4035828888023));
#16624=CARTESIAN_POINT('Ctrl Pts',(84.9983835871451,2.87367749904876,-2.36708773820864));
#16625=CARTESIAN_POINT('Ctrl Pts',(85.0039760887491,2.94245505296496,-2.28138429292121));
#16626=CARTESIAN_POINT('Ctrl Pts',(85.0070887152721,2.98025732090569,-2.23177574181176));
#16627=CARTESIAN_POINT('Ctrl Pts',(85.0185648194923,3.11670618534649,-2.0430579984548));
#16628=CARTESIAN_POINT('Ctrl Pts',(85.0266666177967,3.20700741484958,-1.89817057062981));
#16629=CARTESIAN_POINT('Ctrl Pts',(85.0438943628245,3.37556394950495,-1.58113230508593));
#16630=CARTESIAN_POINT('Ctrl Pts',(85.0530195233058,3.4512890778597,-1.40819302504942));
#16631=CARTESIAN_POINT('Ctrl Pts',(85.0660109939238,3.53621385168474,-1.16565301833298));
#16632=CARTESIAN_POINT('Ctrl Pts',(85.0695210442296,3.55705261892887,-1.10042323551924));
#16633=CARTESIAN_POINT('Ctrl Pts',(85.0754655470594,3.58876800525969,-0.99080563590118));
#16634=CARTESIAN_POINT('Ctrl Pts',(85.0778680993223,3.60064770608313,-0.946724595775906));
#16635=CARTESIAN_POINT('Ctrl Pts',(85.082748123297,3.62288739772546,-0.857717437968567));
#16636=CARTESIAN_POINT('Ctrl Pts',(85.0852256668082,3.63322942484477,-0.81279517157289));
#16637=CARTESIAN_POINT('Ctrl Pts',(85.0915837520213,3.65736948030658,-0.698249743210625));
#16638=CARTESIAN_POINT('Ctrl Pts',(85.095498729564,3.67001506327405,-0.628404912958072));
#16639=CARTESIAN_POINT('Ctrl Pts',(85.1042959845805,3.69358477160547,-0.473003445243937));
#16640=CARTESIAN_POINT('Ctrl Pts',(85.1092029291424,3.70354750565902,-0.387343705000337));
#16641=CARTESIAN_POINT('Ctrl Pts',(85.126596933153,3.72796870382054,-0.0867143048216947));
#16642=CARTESIAN_POINT('Ctrl Pts',(85.1394183000811,3.72674060072934,0.129091739340578));
#16643=CARTESIAN_POINT('Ctrl Pts',(85.1598575977116,3.69463973859095,0.475444047252364));
#16644=CARTESIAN_POINT('Ctrl Pts',(85.1675555825175,3.67538615230655,0.606590205940345));
#16645=CARTESIAN_POINT('Ctrl Pts',(85.1771158314097,3.64161019859385,0.773955767594703));
#16646=CARTESIAN_POINT('Ctrl Pts',(85.179234631196,3.63346062847825,0.811354704571847));
#16647=CARTESIAN_POINT('Ctrl Pts',(85.1826972983423,3.6190005250616,0.873118370521107));
#16648=CARTESIAN_POINT('Ctrl Pts',(85.1840576968601,3.61301723882062,0.897556156096714));
#16649=CARTESIAN_POINT('Ctrl Pts',(85.1869523224538,3.59962106044714,0.94996468101585));
#16650=CARTESIAN_POINT('Ctrl Pts',(85.1884823846651,3.59212910964458,0.977912694539554));
#16651=CARTESIAN_POINT('Ctrl Pts',(85.192967893653,3.568970590119,1.06044373238354));
#16652=CARTESIAN_POINT('Ctrl Pts',(85.1958772412779,3.55237967468349,1.11476062781221));
#16653=CARTESIAN_POINT('Ctrl Pts',(85.2027872708971,3.50936458033948,1.24485541880959));
#16654=CARTESIAN_POINT('Ctrl Pts',(85.2067409966739,3.48172017835727,1.32020093105392));
#16655=CARTESIAN_POINT('Ctrl Pts',(85.2180823766607,3.39444499365084,1.53620909772717));
#16656=CARTESIAN_POINT('Ctrl Pts',(85.2253388973998,3.32856692658448,1.67416827599768));
#16657=CARTESIAN_POINT('Ctrl Pts',(85.2410436683723,3.16989163459986,1.95983227580369));
#16658=CARTESIAN_POINT('Ctrl Pts',(85.2495023220511,3.07482457616018,2.10584967689417));
#16659=CARTESIAN_POINT('Ctrl Pts',(85.2617398911134,2.92893577849752,2.29887327896219));
#16660=CARTESIAN_POINT('Ctrl Pts',(85.2652241509502,2.88649753061265,2.3519384421253));
#16661=CARTESIAN_POINT('Ctrl Pts',(85.2709010511713,2.8161492148612,2.43512902468597));
#16662=CARTESIAN_POINT('Ctrl Pts',(85.2730579411314,2.7891506599999,2.46600652658258));
#16663=CARTESIAN_POINT('Ctrl Pts',(85.2776415935549,2.73125754398276,2.53005012436876));
#16664=CARTESIAN_POINT('Ctrl Pts',(85.280072531138,2.70025654879109,2.56311055782589));
#16665=CARTESIAN_POINT('Ctrl Pts',(85.2861348167576,2.62226764885239,2.64329480692903));
#16666=CARTESIAN_POINT('Ctrl Pts',(85.2897942444364,2.57460635569363,2.68973909696347));
#16667=CARTESIAN_POINT('Ctrl Pts',(85.3034275194096,2.39499752822537,2.85561224541495));
#16668=CARTESIAN_POINT('Ctrl Pts',(85.3137102570149,2.25579212138062,2.96680376765666));
#16669=CARTESIAN_POINT('Ctrl Pts',(85.3390006099171,1.90101237685729,3.21073849834573));
#16670=CARTESIAN_POINT('Ctrl Pts',(85.3541374800096,1.67880840364266,3.33231146350343));
#16671=CARTESIAN_POINT('Ctrl Pts',(85.3709141654963,1.40471472741503,3.44784736342914));
#16672=CARTESIAN_POINT('Ctrl Pts',(85.3734104222247,1.36311660588644,3.46450405866438));
#16673=CARTESIAN_POINT('Ctrl Pts',(85.3773261940875,1.29636051776932,3.48984589578087));
#16674=CARTESIAN_POINT('Ctrl Pts',(85.3787708962779,1.27139350176222,3.49901895286059));
#16675=CARTESIAN_POINT('Ctrl Pts',(85.3816501553886,1.22089448978339,3.51696073440474));
#16676=CARTESIAN_POINT('Ctrl Pts',(85.383084228597,1.1953612431606,3.52572088348676));
#16677=CARTESIAN_POINT('Ctrl Pts',(85.386963405192,1.12534039699767,3.54889606166907));
#16678=CARTESIAN_POINT('Ctrl Pts',(85.3893794862127,1.08067174557414,3.56275219719353));
#16679=CARTESIAN_POINT('Ctrl Pts',(85.4001148621791,0.878228383851434,3.62139173424208));
#16680=CARTESIAN_POINT('Ctrl Pts',(85.4080426475064,0.717848812927682,3.65656459621806));
#16681=CARTESIAN_POINT('Ctrl Pts',(85.428586926304,0.294683416065642,3.72044230909833));
#16682=CARTESIAN_POINT('Ctrl Pts',(85.4411087798052,0.0302761415880997,
3.73197041859556));
#16683=CARTESIAN_POINT('Ctrl Pts',(85.4578286262312,-0.29911254598409,3.71130314038781));
#16684=CARTESIAN_POINT('Ctrl Pts',(85.4612242458891,-0.364977212526694,
3.70540554909866));
#16685=CARTESIAN_POINT('Ctrl Pts',(85.4670090376998,-0.475145527758885,
3.69257514701699));
#16686=CARTESIAN_POINT('Ctrl Pts',(85.4693691721422,-0.519544989957933,
3.68659019485562));
#16687=CARTESIAN_POINT('Ctrl Pts',(85.474229480708,-0.60978872310713,3.67276293703801));
#16688=CARTESIAN_POINT('Ctrl Pts',(85.4767311338216,-0.655615537576436,
3.66485987221069));
#16689=CARTESIAN_POINT('Ctrl Pts',(85.4832395072245,-0.773182520215193,
3.64230921161286));
#16690=CARTESIAN_POINT('Ctrl Pts',(85.487284027,-0.844657878632875,3.62640037271484));
#16691=CARTESIAN_POINT('Ctrl Pts',(85.4964387681904,-1.00292135129857,3.58624170739158));
#16692=CARTESIAN_POINT('Ctrl Pts',(85.5015771493159,-1.08939050622804,3.56092790127404));
#16693=CARTESIAN_POINT('Ctrl Pts',(85.520693131495,-1.40318706911168,3.45656436676044));
#16694=CARTESIAN_POINT('Ctrl Pts',(85.5350869986141,-1.62361723200026,3.35866453585474));
#16695=CARTESIAN_POINT('Ctrl Pts',(85.5551668799099,-1.92313195969921,3.18922337607143));
#16696=CARTESIAN_POINT('Ctrl Pts',(85.5611254427033,-2.0110678368837,3.13451613488043));
#16697=CARTESIAN_POINT('Ctrl Pts',(85.5689260043489,-2.12650198376631,3.0558411414526));
#16698=CARTESIAN_POINT('Ctrl Pts',(85.5709234868712,-2.15609221874516,3.03503580003459));
#16699=CARTESIAN_POINT('Ctrl Pts',(85.5742631658348,-2.20571358658557,2.99905422758009));
#16700=CARTESIAN_POINT('Ctrl Pts',(85.5756188393707,-2.22590215299836,2.98410093884328));
#16701=CARTESIAN_POINT('Ctrl Pts',(85.5785691957999,-2.26995988419176,2.95077224761442));
#16702=CARTESIAN_POINT('Ctrl Pts',(85.5801582371514,-2.2937597757726,2.93230983019852));
#16703=CARTESIAN_POINT('Ctrl Pts',(85.5850429041051,-2.36700938840469,2.87404990181377));
#16704=CARTESIAN_POINT('Ctrl Pts',(85.5882792277949,-2.41566911748086,2.83327369662885));
#16705=CARTESIAN_POINT('Ctrl Pts',(85.5950764191946,-2.51730318488695,2.74358279703725));
#16706=CARTESIAN_POINT('Ctrl Pts',(85.598620270255,-2.56994374939982,2.69433672039096));
#16707=CARTESIAN_POINT('Ctrl Pts',(85.6021262427416,-2.62112000930789,2.64359555516834));
#16708=CARTESIAN_POINT('Origin',(80.1322559480305,0.,0.));
#16709=CARTESIAN_POINT('',(87.0941439883772,-2.62111999291044,2.64359557142638));
#16710=CARTESIAN_POINT('',(86.8469367975669,-2.62112000772923,2.64359555673358));
#16711=CARTESIAN_POINT('',(80.1322559480305,-2.62112000711956,2.64359555733806));
#16712=CARTESIAN_POINT('Ctrl Pts',(87.0941439883772,-2.62111999291044,2.64359557142638));
#16713=CARTESIAN_POINT('Ctrl Pts',(87.091234710344,-2.57927384666699,2.68508594602471));
#16714=CARTESIAN_POINT('Ctrl Pts',(87.0883621998307,-2.53643946225557,2.72558579927331));
#16715=CARTESIAN_POINT('Ctrl Pts',(87.0751689172554,-2.33394346756449,2.9081323252061));
#16716=CARTESIAN_POINT('Ctrl Pts',(87.0650941661905,-2.16321393192004,3.03727380232705));
#16717=CARTESIAN_POINT('Ctrl Pts',(87.0504372145944,-1.90961892014635,3.19681187581807));
#16718=CARTESIAN_POINT('Ctrl Pts',(87.0461806764361,-1.83533027562482,3.24003275801531));
#16719=CARTESIAN_POINT('Ctrl Pts',(87.0382735907821,-1.69722498701445,3.31410732065542));
#16720=CARTESIAN_POINT('Ctrl Pts',(87.0346500589835,-1.63389525245935,3.34578324019333));
#16721=CARTESIAN_POINT('Ctrl Pts',(87.028569442854,-1.52793389649372,3.39505633437968));
#16722=CARTESIAN_POINT('Ctrl Pts',(87.0261476761901,-1.48580888212723,3.4137019825099));
#16723=CARTESIAN_POINT('Ctrl Pts',(87.0212723765704,-1.40124353522606,3.44927104204571));
#16724=CARTESIAN_POINT('Ctrl Pts',(87.0188197000595,-1.35881609967048,3.46620436865924));
#16725=CARTESIAN_POINT('Ctrl Pts',(87.0126182982754,-1.2518944315951,3.50661338693058));
#16726=CARTESIAN_POINT('Ctrl Pts',(87.0088385463976,-1.18704435583023,3.52909364801014));
#16727=CARTESIAN_POINT('Ctrl Pts',(86.9941201512639,-0.93581211070486,3.60847497750482));
#16728=CARTESIAN_POINT('Ctrl Pts',(86.9828048860468,-0.745708861740775,
3.6524976899244));
#16729=CARTESIAN_POINT('Ctrl Pts',(86.9615749957209,-0.389271763427499,
3.7060443984394));
#16730=CARTESIAN_POINT('Ctrl Pts',(86.9517339586807,-0.224028354117965,
3.71969226663774));
#16731=CARTESIAN_POINT('Ctrl Pts',(86.9385603172174,0.00304872113064497,
3.7232563760466));
#16732=CARTESIAN_POINT('Ctrl Pts',(86.9350293986215,0.0645381599798527,
3.72269832176204));
#16733=CARTESIAN_POINT('Ctrl Pts',(86.9288949343423,0.173003292476461,3.71902546379455));
#16734=CARTESIAN_POINT('Ctrl Pts',(86.9262689318477,0.219986391202562,3.71654233430373));
#16735=CARTESIAN_POINT('Ctrl Pts',(86.9222002944552,0.293891133961937,3.71122987822687));
#16736=CARTESIAN_POINT('Ctrl Pts',(86.920729233345,0.320849354963846,3.70899649341275));
#16737=CARTESIAN_POINT('Ctrl Pts',(86.9178463775644,0.374212645525434,3.70398936378226));
#16738=CARTESIAN_POINT('Ctrl Pts',(86.9164341798328,0.400616964721536,3.70122661066823));
#16739=CARTESIAN_POINT('Ctrl Pts',(86.9126895916483,0.471247353124605,3.69307166354918));
#16740=CARTESIAN_POINT('Ctrl Pts',(86.9103828737011,0.515411187451082,3.68716747884026));
#16741=CARTESIAN_POINT('Ctrl Pts',(86.8951303223451,0.810717408010992,3.64227864855071));
#16742=CARTESIAN_POINT('Ctrl Pts',(86.8831861308858,1.05742771334007,3.57845339306033));
#16743=CARTESIAN_POINT('Ctrl Pts',(86.8624562488596,1.46178423452129,3.42832760359663));
#16744=CARTESIAN_POINT('Ctrl Pts',(86.8538445630491,1.6232189039216,3.35490637898227));
#16745=CARTESIAN_POINT('Ctrl Pts',(86.8415102271794,1.83715658282693,3.23853911018966));
#16746=CARTESIAN_POINT('Ctrl Pts',(86.8380996896994,1.89464596396203,3.20524505688366));
#16747=CARTESIAN_POINT('Ctrl Pts',(86.8322737385911,1.98979115161382,3.14668886916404));
#16748=CARTESIAN_POINT('Ctrl Pts',(86.8298873161157,2.02793267179682,3.12224414641387));
#16749=CARTESIAN_POINT('Ctrl Pts',(86.8252910676337,2.09975512704548,3.07434216112538));
#16750=CARTESIAN_POINT('Ctrl Pts',(86.8230860974373,2.13351292703815,3.05101191854651));
#16751=CARTESIAN_POINT('Ctrl Pts',(86.8171692110018,2.22221803790045,2.98751509031372));
#16752=CARTESIAN_POINT('Ctrl Pts',(86.8134222422132,2.27645938652393,2.9463929252939));
#16753=CARTESIAN_POINT('Ctrl Pts',(86.7959460958633,2.52059790445449,2.75053614468384));
#16754=CARTESIAN_POINT('Ctrl Pts',(86.7815736230602,2.69603966561627,2.57879913774977));
#16755=CARTESIAN_POINT('Ctrl Pts',(86.7557831455884,2.976543323531,2.24407201686349));
#16756=CARTESIAN_POINT('Ctrl Pts',(86.7444550819635,3.08821906628995,2.08772183895059));
#16757=CARTESIAN_POINT('Ctrl Pts',(86.7314503638769,3.20798010367828,1.88926584402681));
#16758=CARTESIAN_POINT('Ctrl Pts',(86.7292360530217,3.22805921721248,1.85474950311365));
#16759=CARTESIAN_POINT('Ctrl Pts',(86.7256500133549,3.26013254986333,1.79751568543212));
#16760=CARTESIAN_POINT('Ctrl Pts',(86.724259810935,3.27245364637974,1.77498567652399));
#16761=CARTESIAN_POINT('Ctrl Pts',(86.7213639468827,3.2979008403936,1.72728779473046));
#16762=CARTESIAN_POINT('Ctrl Pts',(86.7198612343079,3.31097391549297,1.70209427154438));
#16763=CARTESIAN_POINT('Ctrl Pts',(86.715552969407,3.34800737589311,1.62868437483962));
#16764=CARTESIAN_POINT('Ctrl Pts',(86.7127881618465,3.3712123098086,1.58009312673608));
#16765=CARTESIAN_POINT('Ctrl Pts',(86.7046950683262,3.43703218331002,1.43420918774034));
#16766=CARTESIAN_POINT('Ctrl Pts',(86.6994914317596,3.47654841031451,1.33557472888027));
#16767=CARTESIAN_POINT('Ctrl Pts',(86.6840090581203,3.5827159194742,1.03377424405145));
#16768=CARTESIAN_POINT('Ctrl Pts',(86.673932548184,3.63614415233331,0.826437651324505));
#16769=CARTESIAN_POINT('Ctrl Pts',(86.6592734084947,3.6856997688977,0.53091331183854));
#16770=CARTESIAN_POINT('Ctrl Pts',(86.6550165598259,3.69697175782733,0.44570220647882));
#16771=CARTESIAN_POINT('Ctrl Pts',(86.6471089674876,3.71213530202019,0.289710271656887));
#16772=CARTESIAN_POINT('Ctrl Pts',(86.6434852456678,3.71697343771286,0.219062096731713));
#16773=CARTESIAN_POINT('Ctrl Pts',(86.6374044008693,3.72162944582098,0.102292904319072));
#16774=CARTESIAN_POINT('Ctrl Pts',(86.6349826013614,3.72261022495269,0.0562355517218713));
#16775=CARTESIAN_POINT('Ctrl Pts',(86.6301073051167,3.72286092596252,-0.0355054231258351));
#16776=CARTESIAN_POINT('Ctrl Pts',(86.6276546663145,3.72214501490199,-0.0811809627238327));
#16777=CARTESIAN_POINT('Ctrl Pts',(86.6214535046793,3.71825097383426,-0.195413189595637));
#16778=CARTESIAN_POINT('Ctrl Pts',(86.6176739603969,3.71401733190922,-0.263914841127556));
#16779=CARTESIAN_POINT('Ctrl Pts',(86.6029653253518,3.69051757253894,-0.526165055799792));
#16780=CARTESIAN_POINT('Ctrl Pts',(86.5916603801591,3.65795985707613,-0.718390179630367));
#16781=CARTESIAN_POINT('Ctrl Pts',(86.5704332110095,3.57013733808099,-1.06792337880992));
#16782=CARTESIAN_POINT('Ctrl Pts',(86.5605842079323,3.5190553710567,-1.22580256063017));
#16783=CARTESIAN_POINT('Ctrl Pts',(86.5474013957484,3.43482667150271,-1.43687716921547));
#16784=CARTESIAN_POINT('Ctrl Pts',(86.5438690545387,3.41061861836088,-1.49342945457998));
#16785=CARTESIAN_POINT('Ctrl Pts',(86.5377324247055,3.36543564296836,-1.5921446892173));
#16786=CARTESIAN_POINT('Ctrl Pts',(86.5351056586267,3.34504142930956,-1.63455804739113));
#16787=CARTESIAN_POINT('Ctrl Pts',(86.531036123131,3.31166474033107,-1.7007280788922));
#16788=CARTESIAN_POINT('Ctrl Pts',(86.5295649079841,3.29921853093252,-1.72474824972293));
#16789=CARTESIAN_POINT('Ctrl Pts',(86.5266820181287,3.27404275807684,-1.77206551926204));
#16790=CARTESIAN_POINT('Ctrl Pts',(86.525269935454,3.26132372346861,-1.79536620823842));
#16791=CARTESIAN_POINT('Ctrl Pts',(86.521526061774,3.22659910322151,-1.85739321627774));
#16792=CARTESIAN_POINT('Ctrl Pts',(86.5192199257933,3.20414532689804,-1.89586507586917));
#16793=CARTESIAN_POINT('Ctrl Pts',(86.503964144065,3.04894413769073,-2.15114671041387));
#16794=CARTESIAN_POINT('Ctrl Pts',(86.4920168411387,2.89496739083631,-2.35429011359411));
#16795=CARTESIAN_POINT('Ctrl Pts',(86.4712852251985,2.60063532172118,-2.6696303005918));
#16796=CARTESIAN_POINT('Ctrl Pts',(86.4626752456974,2.47072070710897,-2.7902978916309));
#16797=CARTESIAN_POINT('Ctrl Pts',(86.4503430188948,2.28095743290653,-2.94287484692372));
#16798=CARTESIAN_POINT('Ctrl Pts',(86.4469327394015,2.22809189548189,-2.98309989879739));
#16799=CARTESIAN_POINT('Ctrl Pts',(86.4411070955824,2.13740957935147,-3.04834379191097));
#16800=CARTESIAN_POINT('Ctrl Pts',(86.4387207150123,2.10015989208887,-3.07412553030201));
#16801=CARTESIAN_POINT('Ctrl Pts',(86.4341244595709,2.02828856245078,-3.12195401847443));
#16802=CARTESIAN_POINT('Ctrl Pts',(86.4319194386632,1.99375449651386,-3.14412057869629));
#16803=CARTESIAN_POINT('Ctrl Pts',(86.426002195275,1.90098311538947,-3.20152516143294));
#16804=CARTESIAN_POINT('Ctrl Pts',(86.4222549122829,1.84213575449728,-3.23574337857887));
#16805=CARTESIAN_POINT('Ctrl Pts',(86.4085932330683,1.62732783423568,-3.35288909819996));
#16806=CARTESIAN_POINT('Ctrl Pts',(86.3983796386424,1.46646432188542,-3.42630007277247));
#16807=CARTESIAN_POINT('Ctrl Pts',(86.3774232449251,1.13228802828112,-3.55094642527077));
#16808=CARTESIAN_POINT('Ctrl Pts',(86.3667023622961,0.959218475685186,-3.60155484728061));
#16809=CARTESIAN_POINT('Ctrl Pts',(86.3508705634862,0.692808651888334,-3.65888318765684));
#16810=CARTESIAN_POINT('Ctrl Pts',(86.345577330563,0.60175253614416,-3.67495662261087));
#16811=CARTESIAN_POINT('Ctrl Pts',(86.3385235647833,0.476277003299358,-3.69231630235341));
#16812=CARTESIAN_POINT('Ctrl Pts',(86.3366376564716,0.442302673423051,-3.6965400002081));
#16813=CARTESIAN_POINT('Ctrl Pts',(86.3334193235122,0.383478668138524,-3.70303037436475));
#16814=CARTESIAN_POINT('Ctrl Pts',(86.3320759896681,0.358656856810983,-3.70551685988385));
#16815=CARTESIAN_POINT('Ctrl Pts',(86.3290711156063,0.302512163386443,-3.71057157847395));
#16816=CARTESIAN_POINT('Ctrl Pts',(86.3274170929586,0.27117901036536,-3.71299301401829));
#16817=CARTESIAN_POINT('Ctrl Pts',(86.322058361885,0.168444805649324,-3.71962488191335));
#16818=CARTESIAN_POINT('Ctrl Pts',(86.3184307732184,0.0969495923947637,
-3.72217474645538));
#16819=CARTESIAN_POINT('Ctrl Pts',(86.301140067071,-0.249946241598828,-3.72454364688135));
#16820=CARTESIAN_POINT('Ctrl Pts',(86.2883343425865,-0.524685446967067,
-3.69586571150935));
#16821=CARTESIAN_POINT('Ctrl Pts',(86.2703371553668,-0.885919711062651,
-3.61703073702839));
#16822=CARTESIAN_POINT('Ctrl Pts',(86.2656890673109,-0.977275751649216,
-3.5934239723411));
#16823=CARTESIAN_POINT('Ctrl Pts',(86.2571471206628,-1.14008979882564,-3.54468379837117));
#16824=CARTESIAN_POINT('Ctrl Pts',(86.2532885893692,-1.21186497192525,-3.52079114814455));
#16825=CARTESIAN_POINT('Ctrl Pts',(86.2469241736505,-1.32692718729817,-3.47855363718965));
#16826=CARTESIAN_POINT('Ctrl Pts',(86.244461049937,-1.37068320718194,-3.46154567407277));
#16827=CARTESIAN_POINT('Ctrl Pts',(86.239609245014,-1.4552856064792,-3.42680509958048));
#16828=CARTESIAN_POINT('Ctrl Pts',(86.2372236896611,-1.49615860917684,-3.40915804466471));
#16829=CARTESIAN_POINT('Ctrl Pts',(86.2313283567601,-1.59534948342596,-3.36420469838027));
#16830=CARTESIAN_POINT('Ctrl Pts',(86.2277929668989,-1.65329272174107,-3.3361108661339));
#16831=CARTESIAN_POINT('Ctrl Pts',(86.2087679124266,-1.95690823409506,-3.17904981015634));
#16832=CARTESIAN_POINT('Ctrl Pts',(86.1924049772516,-2.18828718485437,-3.02443480990461));
#16833=CARTESIAN_POINT('Ctrl Pts',(86.1692538297488,-2.48817075252099,-2.7714772367783));
#16834=CARTESIAN_POINT('Ctrl Pts',(86.1624958015562,-2.57255569733065,-2.69333232559858));
#16835=CARTESIAN_POINT('Ctrl Pts',(86.152967932467,-2.68870537949301,-2.57532405589478));
#16836=CARTESIAN_POINT('Ctrl Pts',(86.1500838301582,-2.72348020859216,-2.53852054599982));
#16837=CARTESIAN_POINT('Ctrl Pts',(86.1449484390948,-2.78491047515975,-2.47079066460091));
#16838=CARTESIAN_POINT('Ctrl Pts',(86.1426832719786,-2.81182843066204,-2.44011352379744));
#16839=CARTESIAN_POINT('Ctrl Pts',(86.1390382580498,-2.85495351897188,-2.38930434658693));
#16840=CARTESIAN_POINT('Ctrl Pts',(86.1376387504644,-2.87146476911752,-2.36943560180076));
#16841=CARTESIAN_POINT('Ctrl Pts',(86.1347492572674,-2.90548701794336,-2.32761701889195));
#16842=CARTESIAN_POINT('Ctrl Pts',(86.1332617095365,-2.92295885611954,-2.30563818066895));
#16843=CARTESIAN_POINT('Ctrl Pts',(86.1290499348558,-2.97222482089685,-2.24220345840253));
#16844=CARTESIAN_POINT('Ctrl Pts',(86.1263636662157,-3.00339819035779,-2.20027192596006));
#16845=CARTESIAN_POINT('Ctrl Pts',(86.1108641311429,-3.18077738182521,-1.95088014821582));
#16846=CARTESIAN_POINT('Ctrl Pts',(86.0989638794391,-3.30635261652344,-1.72954705126819));
#16847=CARTESIAN_POINT('Ctrl Pts',(86.0809297235219,-3.45697624840952,-1.3866330424685));
#16848=CARTESIAN_POINT('Ctrl Pts',(86.0750632668744,-3.5001117929979,-1.27383329321157));
#16849=CARTESIAN_POINT('Ctrl Pts',(86.0646014739261,-3.56554401578721,-1.07413475770021));
#16850=CARTESIAN_POINT('Ctrl Pts',(86.0600743652014,-3.59032260376837,-0.988155706948785));
#16851=CARTESIAN_POINT('Ctrl Pts',(86.0528974291893,-3.62395109652917,-0.853399459939284));
#16852=CARTESIAN_POINT('Ctrl Pts',(86.050314465975,-3.63496525114363,-0.805195325660149));
#16853=CARTESIAN_POINT('Ctrl Pts',(86.0453711446694,-3.65398003992337,-0.713611886942932));
#16854=CARTESIAN_POINT('Ctrl Pts',(86.0430173192182,-3.66217617058866,-0.670281680117861));
#16855=CARTESIAN_POINT('Ctrl Pts',(86.0375558301385,-3.67922967059822,-0.570444723274658));
#16856=CARTESIAN_POINT('Ctrl Pts',(86.0344325619859,-3.68755820915327,-0.513860017721723));
#16857=CARTESIAN_POINT('Ctrl Pts',(86.023593687396,-3.71162884604093,-0.319308837833603));
#16858=CARTESIAN_POINT('Ctrl Pts',(86.0156928360809,-3.72095373050056,-0.180676435058985));
#16859=CARTESIAN_POINT('Ctrl Pts',(86.0067692681638,-3.722682803568,-0.0269054678282001));
#16860=CARTESIAN_POINT('Ctrl Pts',(86.0058999202337,-3.72276084300876,-0.0119524458300203));
#16861=CARTESIAN_POINT('Ctrl Pts',(85.9967740637689,-3.72263454584351,0.144742773224368));
#16862=CARTESIAN_POINT('Ctrl Pts',(85.9883845617901,-3.7144251989962,0.28635919450188));
#16863=CARTESIAN_POINT('Ctrl Pts',(85.9709413541588,-3.68050254699941,0.580048373103257));
#16864=CARTESIAN_POINT('Ctrl Pts',(85.9619087842773,-3.65337723218817,0.731707651111109));
#16865=CARTESIAN_POINT('Ctrl Pts',(85.9506415789239,-3.60612838185203,0.925630172085175));
#16866=CARTESIAN_POINT('Ctrl Pts',(85.9480952434709,-3.59450172037099,0.969799396397021));
#16867=CARTESIAN_POINT('Ctrl Pts',(85.9441204514966,-3.5747746464447,1.03950492607714));
#16868=CARTESIAN_POINT('Ctrl Pts',(85.9426655759653,-3.567206653127,1.06518592101018));
#16869=CARTESIAN_POINT('Ctrl Pts',(85.939785552781,-3.5515070010549,1.11641582106765));
#16870=CARTESIAN_POINT('Ctrl Pts',(85.9383605269914,-3.54337506691927,1.14196299637133));
#16871=CARTESIAN_POINT('Ctrl Pts',(85.9345367812972,-3.52058880253859,1.21096014234923));
#16872=CARTESIAN_POINT('Ctrl Pts',(85.932165692308,-3.50540619694783,1.25423192944197));
#16873=CARTESIAN_POINT('Ctrl Pts',(85.9218857338454,-3.4351509638238,1.44321427556931));
#16874=CARTESIAN_POINT('Ctrl Pts',(85.9143313362934,-3.37176042436534,1.5856760974596));
#16875=CARTESIAN_POINT('Ctrl Pts',(85.8934922586439,-3.17099912689698,1.96997476260508));
#16876=CARTESIAN_POINT('Ctrl Pts',(85.8803546562412,-3.01522915536588,2.20100433970703));
#16877=CARTESIAN_POINT('Ctrl Pts',(85.8629942517555,-2.79352059610721,2.46155427520549));
#16878=CARTESIAN_POINT('Ctrl Pts',(85.8596855616872,-2.75056527281446,2.50946146266941));
#16879=CARTESIAN_POINT('Ctrl Pts',(85.8542022108891,-2.67844635242311,2.58581689865048));
#16880=CARTESIAN_POINT('Ctrl Pts',(85.8520579517535,-2.6500186227414,2.61494263447641));
#16881=CARTESIAN_POINT('Ctrl Pts',(85.8498933978769,-2.62112000707361,2.64359555738363));
#16882=CARTESIAN_POINT('',(85.760341149807,-3.72274987726766,-0.000955930746860748));
#16883=CARTESIAN_POINT('Ctrl Pts',(85.6021262427416,-2.62112000930789,2.64359555516834));
#16884=CARTESIAN_POINT('Ctrl Pts',(85.6032237479712,-2.63714016151762,2.62771160445319));
#16885=CARTESIAN_POINT('Ctrl Pts',(85.6043175234224,-2.65301682263349,2.611681144791));
#16886=CARTESIAN_POINT('Ctrl Pts',(85.6204504607634,-2.88564119772402,2.37249240765257));
#16887=CARTESIAN_POINT('Ctrl Pts',(85.6350064317477,-3.07371361545918,2.12318795058449));
#16888=CARTESIAN_POINT('Ctrl Pts',(85.6540442114052,-3.26042230954893,1.79794384197059));
#16889=CARTESIAN_POINT('Ctrl Pts',(85.6573334774966,-3.2908193617108,1.74168395999376));
#16890=CARTESIAN_POINT('Ctrl Pts',(85.6629930620253,-3.3398653990825,1.64503563015123));
#16891=CARTESIAN_POINT('Ctrl Pts',(85.6653373612563,-3.35926718323422,1.6050441979263));
#16892=CARTESIAN_POINT('Ctrl Pts',(85.670214350167,-3.39773133500175,1.52200683470502));
#16893=CARTESIAN_POINT('Ctrl Pts',(85.67274954924,-3.41670246926471,1.47892764998727));
#16894=CARTESIAN_POINT('Ctrl Pts',(85.6794664790305,-3.46428138622222,1.3650813849668));
#16895=CARTESIAN_POINT('Ctrl Pts',(85.683690847758,-3.49153746178149,1.29377653654447));
#16896=CARTESIAN_POINT('Ctrl Pts',(85.696816072913,-3.56818137717465,1.07315993754611));
#16897=CARTESIAN_POINT('Ctrl Pts',(85.7059206556922,-3.61031497043406,0.921525182771377));
#16898=CARTESIAN_POINT('Ctrl Pts',(85.7220082984104,-3.6668019232921,0.653492386157504));
#16899=CARTESIAN_POINT('Ctrl Pts',(85.7289222746521,-3.68548553613412,0.538223500814585));
#16900=CARTESIAN_POINT('Ctrl Pts',(85.744125487982,-3.7147635344508,0.281772912376273));
#16901=CARTESIAN_POINT('Ctrl Pts',(85.7523850009167,-3.72278619233908,0.140468464394411));
#16902=CARTESIAN_POINT('Ctrl Pts',(85.760341149807,-3.72274987726766,-0.000955930746860748));
#16903=CARTESIAN_POINT('Ctrl Pts',(85.7603413601859,-3.72274987630553,-0.000959670334727729));
#16904=CARTESIAN_POINT('Ctrl Pts',(85.7620234535716,-3.72274216851247,-0.0308597147720175));
#16905=CARTESIAN_POINT('Ctrl Pts',(85.7636914883015,-3.72237423781889,-0.0607595695636158));
#16906=CARTESIAN_POINT('Ctrl Pts',(85.76688002092,-3.7209684279052,-0.118473539850565));
#16907=CARTESIAN_POINT('Ctrl Pts',(85.7684026300494,-3.71997880335005,-0.146286764873807));
#16908=CARTESIAN_POINT('Ctrl Pts',(85.7712404249104,-3.7175267093758,-0.198665983594152));
#16909=CARTESIAN_POINT('Ctrl Pts',(85.7725586100737,-3.71613249638555,-0.223231507567389));
#16910=CARTESIAN_POINT('Ctrl Pts',(85.7757422062399,-3.71213868356963,-0.283102350288278));
#16911=CARTESIAN_POINT('Ctrl Pts',(85.7775942166989,-3.70927894502006,-0.318387237437441));
#16912=CARTESIAN_POINT('Ctrl Pts',(85.7844257586302,-3.69672585713205,-0.449940163380343));
#16913=CARTESIAN_POINT('Ctrl Pts',(85.7892606494674,-3.68378367955504,-0.545864913335448));
#16914=CARTESIAN_POINT('Ctrl Pts',(85.7990812631252,-3.64931792670788,-0.742985128920719));
#16915=CARTESIAN_POINT('Ctrl Pts',(85.8040509119715,-3.62728600636354,-0.844005746828899));
#16916=CARTESIAN_POINT('Ctrl Pts',(85.8202961752315,-3.54137552192721,-1.17173517848588));
#16917=CARTESIAN_POINT('Ctrl Pts',(85.8315127254487,-3.46020168281947,-1.39330549026171));
#16918=CARTESIAN_POINT('Ctrl Pts',(85.8470625877511,-3.32698661590936,-1.67195036076543));
#16919=CARTESIAN_POINT('Ctrl Pts',(85.8508135674605,-3.29336800030353,-1.73723466447043));
#16920=CARTESIAN_POINT('Ctrl Pts',(85.857047842864,-3.23532216759319,-1.84220624266304));
#16921=CARTESIAN_POINT('Ctrl Pts',(85.8594918470563,-3.21204081089915,-1.88250549660204));
#16922=CARTESIAN_POINT('Ctrl Pts',(85.8643393894678,-3.16489124281644,-1.96069771704336));
#16923=CARTESIAN_POINT('Ctrl Pts',(85.8667405411498,-3.1410826432328,-1.99861744991541));
#16924=CARTESIAN_POINT('Ctrl Pts',(85.8727399514875,-3.08052086891813,-2.09131763751415));
#16925=CARTESIAN_POINT('Ctrl Pts',(85.8763659832838,-3.04298558571128,-2.14556665408895));
#16926=CARTESIAN_POINT('Ctrl Pts',(85.8948271741709,-2.84734745166465,-2.41285163066821));
#16927=CARTESIAN_POINT('Ctrl Pts',(85.9104440100743,-2.66825050866978,-2.60952949688887));
#16928=CARTESIAN_POINT('Ctrl Pts',(85.935734866639,-2.34770975351193,-2.89374428403784));
#16929=CARTESIAN_POINT('Ctrl Pts',(85.9453366356581,-2.21861468461013,-2.99386917826029));
#16930=CARTESIAN_POINT('Ctrl Pts',(85.9571958935502,-2.04467801529147,-3.11132412937402));
#16931=CARTESIAN_POINT('Ctrl Pts',(85.9598005404815,-2.00550769109523,-3.13671568879983));
#16932=CARTESIAN_POINT('Ctrl Pts',(85.9638440435153,-1.94296154583124,-3.17560948967413));
#16933=CARTESIAN_POINT('Ctrl Pts',(85.9653107824337,-1.9198996996016,-3.18960505884037));
#16934=CARTESIAN_POINT('Ctrl Pts',(85.9681927067859,-1.87378667581422,-3.21690835070137));
#16935=CARTESIAN_POINT('Ctrl Pts',(85.9696081575552,-1.85074096599047,-3.23022194134742));
#16936=CARTESIAN_POINT('Ctrl Pts',(85.9733729641343,-1.78845064798734,-3.26532179316026));
#16937=CARTESIAN_POINT('Ctrl Pts',(85.9756961504816,-1.74895045960043,-3.28664795176947));
#16938=CARTESIAN_POINT('Ctrl Pts',(85.9908566233137,-1.48508951218564,-3.4230019596901));
#16939=CARTESIAN_POINT('Ctrl Pts',(86.0027120691318,-1.2499058347712,-3.5157067042161));
#16940=CARTESIAN_POINT('Ctrl Pts',(86.0233928514973,-0.835575438296182,
-3.6321397446596));
#16941=CARTESIAN_POINT('Ctrl Pts',(86.0320534234354,-0.660783337843969,
-3.66796726675853));
#16942=CARTESIAN_POINT('Ctrl Pts',(86.0444481643793,-0.418097803460161,
-3.69979650167523));
#16943=CARTESIAN_POINT('Ctrl Pts',(86.0478660498463,-0.351869546893273,
-3.70668140932236));
#16944=CARTESIAN_POINT('Ctrl Pts',(86.0537007272735,-0.240302472715328,
-3.71526266943368));
#16945=CARTESIAN_POINT('Ctrl Pts',(86.0560883160667,-0.1950519291564,-3.71791292133806));
#16946=CARTESIAN_POINT('Ctrl Pts',(86.0606842997619,-0.10878972891976,-3.72138604485015));
#16947=CARTESIAN_POINT('Ctrl Pts',(86.0628877860286,-0.0677906345396503,
-3.72235860038369));
#16948=CARTESIAN_POINT('Ctrl Pts',(86.0687943725394,0.0411142919451229,
-3.72314218317815));
#16949=CARTESIAN_POINT('Ctrl Pts',(86.0725322973588,0.109010882290738,-3.7217729538625));
#16950=CARTESIAN_POINT('Ctrl Pts',(86.0859941946651,0.349868263769225,-3.71031938976274));
#16951=CARTESIAN_POINT('Ctrl Pts',(86.0960040874057,0.522104565570314,-3.69002354922952));
#16952=CARTESIAN_POINT('Ctrl Pts',(86.1169158849143,0.871997688471396,-3.62380193433515));
#16953=CARTESIAN_POINT('Ctrl Pts',(86.1278082882364,1.04895678266236,-3.57659203051134));
#16954=CARTESIAN_POINT('Ctrl Pts',(86.1421829947364,1.28261672762166,-3.49541365849707));
#16955=CARTESIAN_POINT('Ctrl Pts',(86.145892044404,1.34294717522115,-3.47268137084953));
#16956=CARTESIAN_POINT('Ctrl Pts',(86.1522966317303,1.44774544907876,-3.4300539012389));
#16957=CARTESIAN_POINT('Ctrl Pts',(86.1550172664346,1.49246975370475,-3.41083144091072));
#16958=CARTESIAN_POINT('Ctrl Pts',(86.1591970822581,1.56174016449165,-3.37943555025224));
#16959=CARTESIAN_POINT('Ctrl Pts',(86.1606871428466,1.58654952875076,-3.36785950782387));
#16960=CARTESIAN_POINT('Ctrl Pts',(86.163575463146,1.63492219692241,-3.34463565947165));
#16961=CARTESIAN_POINT('Ctrl Pts',(86.1649747153636,1.65849393953887,-3.33301007837422));
#16962=CARTESIAN_POINT('Ctrl Pts',(86.1686375129399,1.72048199199379,-3.30161712757996));
#16963=CARTESIAN_POINT('Ctrl Pts',(86.170877374298,1.75868186846619,-3.28142839792383));
#16964=CARTESIAN_POINT('Ctrl Pts',(86.1844793401716,1.99161226348869,-3.15308772075165));
#16965=CARTESIAN_POINT('Ctrl Pts',(86.1950623158639,2.1766796335749,-3.02829427964438));
#16966=CARTESIAN_POINT('Ctrl Pts',(86.2149102775699,2.49793099866395,-2.76691691646907));
#16967=CARTESIAN_POINT('Ctrl Pts',(86.2241218163708,2.63683101099577,-2.6348821878027));
#16968=CARTESIAN_POINT('Ctrl Pts',(86.2375616561667,2.81595671069249,-2.43619702705285));
#16969=CARTESIAN_POINT('Ctrl Pts',(86.2414458247611,2.86520441335654,-2.37808133623507));
#16970=CARTESIAN_POINT('Ctrl Pts',(86.2478413105384,2.94192893452935,-2.28169551067491));
#16971=CARTESIAN_POINT('Ctrl Pts',(86.2503090240149,2.97052353873976,-2.24434175306066));
#16972=CARTESIAN_POINT('Ctrl Pts',(86.2551622335661,3.02475509317736,-2.17064533606917));
#16973=CARTESIAN_POINT('Ctrl Pts',(86.2575444336255,3.0504637852163,-2.13436524874363));
#16974=CARTESIAN_POINT('Ctrl Pts',(86.2634170036499,3.11160101309343,-2.04472688812219));
#16975=CARTESIAN_POINT('Ctrl Pts',(86.266932517595,3.1463133572091,-1.99089941704815));
#16976=CARTESIAN_POINT('Ctrl Pts',(86.2860730502175,3.32523753254829,-1.69707180038417));
#16977=CARTESIAN_POINT('Ctrl Pts',(86.3025911836158,3.443396601791,-1.44230204935577));
#16978=CARTESIAN_POINT('Ctrl Pts',(86.3282244210372,3.58071922993454,-1.03014355809153));
#16979=CARTESIAN_POINT('Ctrl Pts',(86.3372947884107,3.62039237270546,-0.880631157919389));
#16980=CARTESIAN_POINT('Ctrl Pts',(86.3485998406114,3.65961157650132,-0.684251546319924));
#16981=CARTESIAN_POINT('Ctrl Pts',(86.3511486792379,3.66773784123743,-0.639262515341313));
#16982=CARTESIAN_POINT('Ctrl Pts',(86.3551264232466,3.67930772910303,-0.567696545590053));
#16983=CARTESIAN_POINT('Ctrl Pts',(86.3565818095862,3.68329644110635,-0.541213587991543));
#16984=CARTESIAN_POINT('Ctrl Pts',(86.3592843674836,3.69024773637019,-0.491417663395994));
#16985=CARTESIAN_POINT('Ctrl Pts',(86.3605351246982,3.69327601590024,-0.468115375054028));
#16986=CARTESIAN_POINT('Ctrl Pts',(86.3639931650483,3.70110737538778,-0.40303823657074));
#16987=CARTESIAN_POINT('Ctrl Pts',(86.3661758424477,3.70542375302013,-0.361207304695409));
#16988=CARTESIAN_POINT('Ctrl Pts',(86.3802643899425,3.72901730998095,-0.0871505492183481));
#16989=CARTESIAN_POINT('Ctrl Pts',(86.3913041578462,3.72716444645251,0.146396748049796));
#16990=CARTESIAN_POINT('Ctrl Pts',(86.4113663761407,3.68464715923591,0.562681725536755));
#16991=CARTESIAN_POINT('Ctrl Pts',(86.4203093137164,3.6520619638395,0.745434379651789));
#16992=CARTESIAN_POINT('Ctrl Pts',(86.4334050378777,3.58734939395829,0.997711559086204));
#16993=CARTESIAN_POINT('Ctrl Pts',(86.4372365227098,3.56650049101604,1.06984921147692));
#16994=CARTESIAN_POINT('Ctrl Pts',(86.4435681799452,3.52912561627286,1.18588953662559));
#16995=CARTESIAN_POINT('Ctrl Pts',(86.4460264742298,3.51392567600013,1.23019823383819));
#16996=CARTESIAN_POINT('Ctrl Pts',(86.450876953624,3.48263637006645,1.31609218449873));
#16997=CARTESIAN_POINT('Ctrl Pts',(86.4532661948277,3.46662792376517,1.35769854230954));
#16998=CARTESIAN_POINT('Ctrl Pts',(86.4591863604072,3.42553886425975,1.45902202667711));
#16999=CARTESIAN_POINT('Ctrl Pts',(86.4627434096578,3.39964022229376,1.51838975231757));
#17000=CARTESIAN_POINT('Ctrl Pts',(86.481639946389,3.25585836254753,1.8258387388197));
#17001=CARTESIAN_POINT('Ctrl Pts',(86.4978310497067,3.11234808391068,2.06095867065574));
#17002=CARTESIAN_POINT('Ctrl Pts',(86.5233365058518,2.84788282936661,2.40276217430003));
#17003=CARTESIAN_POINT('Ctrl Pts',(86.5325948236028,2.74362166504506,2.52116029461058));
#17004=CARTESIAN_POINT('Ctrl Pts',(86.5440963871367,2.59959336221692,2.66516477096101));
#17005=CARTESIAN_POINT('Ctrl Pts',(86.5466653289905,2.56641970265719,2.69712424419947));
#17006=CARTESIAN_POINT('Ctrl Pts',(86.5506667729415,2.51298107348377,2.74672798542203));
#17007=CARTESIAN_POINT('Ctrl Pts',(86.5521262577413,2.49310441463993,2.76478190218471));
#17008=CARTESIAN_POINT('Ctrl Pts',(86.554830556129,2.45550528287414,2.79819786430433));
#17009=CARTESIAN_POINT('Ctrl Pts',(86.5560790601752,2.43782975636516,2.81361042350881));
#17010=CARTESIAN_POINT('Ctrl Pts',(86.5595208583163,2.38826573539713,2.85601110524603));
#17011=CARTESIAN_POINT('Ctrl Pts',(86.5616899420457,2.35606601929198,2.88263175694308));
#17012=CARTESIAN_POINT('Ctrl Pts',(86.5758910133389,2.13950242357816,3.05561900446099));
#17013=CARTESIAN_POINT('Ctrl Pts',(86.5870359720157,1.9420426417751,3.18477167842611));
#17014=CARTESIAN_POINT('Ctrl Pts',(86.605137737773,1.60796292594034,3.36058149117198));
#17015=CARTESIAN_POINT('Ctrl Pts',(86.6119821133482,1.47855502271591,3.41949194176839));
#17016=CARTESIAN_POINT('Ctrl Pts',(86.6239254862094,1.2535966770716,3.50673741837284));
#17017=CARTESIAN_POINT('Ctrl Pts',(86.6289220125222,1.15969929668677,3.53889919546114));
#17018=CARTESIAN_POINT('Ctrl Pts',(86.6366686039045,1.01566139621753,3.5818865699422));
#17019=CARTESIAN_POINT('Ctrl Pts',(86.6393321115707,0.966394888843101,3.59549163024325));
#17020=CARTESIAN_POINT('Ctrl Pts',(86.6443405364,0.874362294776768,3.61887846000264));
#17021=CARTESIAN_POINT('Ctrl Pts',(86.6466766216492,0.831672942870827,3.62892692526664));
#17022=CARTESIAN_POINT('Ctrl Pts',(86.6520221336373,0.734590381361373,3.64997579623659));
#17023=CARTESIAN_POINT('Ctrl Pts',(86.6550451322229,0.680109597594471,3.66051865597117));
#17024=CARTESIAN_POINT('Ctrl Pts',(86.6647392334136,0.506811020099884,3.69005226359779));
#17025=CARTESIAN_POINT('Ctrl Pts',(86.6715426127137,0.387306129039432,3.70450171178061));
#17026=CARTESIAN_POINT('Ctrl Pts',(86.691204920197,0.0470238711182816,3.72899959982192));
#17027=CARTESIAN_POINT('Ctrl Pts',(86.7043586670008,-0.174238238734954,
3.72522208861027));
#17028=CARTESIAN_POINT('Ctrl Pts',(86.7249932877825,-0.52362397347469,3.68805096152193));
#17029=CARTESIAN_POINT('Ctrl Pts',(86.7325713348379,-0.652601836679468,
3.6674266045557));
#17030=CARTESIAN_POINT('Ctrl Pts',(86.7419781716467,-0.817009135104777,
3.63218637583907));
#17031=CARTESIAN_POINT('Ctrl Pts',(86.7440585210913,-0.85366008750314,3.62374757216707));
#17032=CARTESIAN_POINT('Ctrl Pts',(86.7474911170056,-0.914753134087983,
3.60870265019284));
#17033=CARTESIAN_POINT('Ctrl Pts',(86.7488587425677,-0.939266452442896,
3.60240014129813));
#17034=CARTESIAN_POINT('Ctrl Pts',(86.7517819567075,-0.992070882991982,
3.58824813995246));
#17035=CARTESIAN_POINT('Ctrl Pts',(86.7533330500894,-1.02033642176015,3.58031326083735));
#17036=CARTESIAN_POINT('Ctrl Pts',(86.7579579721765,-1.10522389961378,3.55539614999773));
#17037=CARTESIAN_POINT('Ctrl Pts',(86.7609812735936,-1.16154009995532,3.53739833012533));
#17038=CARTESIAN_POINT('Ctrl Pts',(86.7763149980169,-1.44946985022717,3.43776190115447));
#17039=CARTESIAN_POINT('Ctrl Pts',(86.7878380537975,-1.67303480865425,3.33468781785303));
#17040=CARTESIAN_POINT('Ctrl Pts',(86.8081604031828,-2.03683335923394,3.12109691305108));
#17041=CARTESIAN_POINT('Ctrl Pts',(86.8167775148827,-2.18229433312326,3.02117856833808));
#17042=CARTESIAN_POINT('Ctrl Pts',(86.8288131620099,-2.36695051414137,2.87402130040385));
#17043=CARTESIAN_POINT('Ctrl Pts',(86.8319043403277,-2.41287001940151,2.835579470552));
#17044=CARTESIAN_POINT('Ctrl Pts',(86.8373580951998,-2.49111325561623,2.76680046078543));
#17045=CARTESIAN_POINT('Ctrl Pts',(86.8397005235802,-2.52385988236031,2.73696202284962));
#17046=CARTESIAN_POINT('Ctrl Pts',(86.8436793063366,-2.57800553040469,2.68582682802946));
#17047=CARTESIAN_POINT('Ctrl Pts',(86.8453025273368,-2.59969198180257,2.66484140401889));
#17048=CARTESIAN_POINT('Ctrl Pts',(86.8469367975669,-2.62112000772923,2.64359555673358));
#17049=CARTESIAN_POINT('Origin',(80.1322559480305,0.,0.));
#17050=CARTESIAN_POINT('',(88.3477258555205,-2.62111983094262,2.64359573201716));
#17051=CARTESIAN_POINT('',(88.1029424526342,-2.62112000712061,2.64359555733703));
#17052=CARTESIAN_POINT('',(80.1322559480305,-2.62112000711956,2.64359555733806));
#17053=CARTESIAN_POINT('',(87.2551002656951,-3.72274852255099,-0.00283400709896036));
#17054=CARTESIAN_POINT('Ctrl Pts',(88.3477258555205,-2.62111983094262,2.64359573201716));
#17055=CARTESIAN_POINT('Ctrl Pts',(88.3386778175898,-2.51136572793979,2.75241670355373));
#17056=CARTESIAN_POINT('Ctrl Pts',(88.3294954746967,-2.39490245454868,2.85433544673622));
#17057=CARTESIAN_POINT('Ctrl Pts',(88.3127086086782,-2.16856793729687,3.028755955785));
#17058=CARTESIAN_POINT('Ctrl Pts',(88.3050930888711,-2.06057942350332,3.10323493620186));
#17059=CARTESIAN_POINT('Ctrl Pts',(88.2956136740075,-1.91632525836319,3.19186856815039));
#17060=CARTESIAN_POINT('Ctrl Pts',(88.2934985649453,-1.88346346357205,3.21136934331982));
#17061=CARTESIAN_POINT('Ctrl Pts',(88.2900265925673,-1.82826926324478,3.24298381229709));
#17062=CARTESIAN_POINT('Ctrl Pts',(88.2886535466726,-1.8061031379439,3.25538079131257));
#17063=CARTESIAN_POINT('Ctrl Pts',(88.2857395313557,-1.75829408664224,3.28148054746855));
#17064=CARTESIAN_POINT('Ctrl Pts',(88.2842026200638,-1.73261475687405,3.29511136209604));
#17065=CARTESIAN_POINT('Ctrl Pts',(88.2796716999771,-1.65563960978507,3.33482175159534));
#17066=CARTESIAN_POINT('Ctrl Pts',(88.2767252181063,-1.60389428165307,3.36001524042488));
#17067=CARTESIAN_POINT('Ctrl Pts',(88.2697028087483,-1.47722902258046,3.41809197960814));
#17068=CARTESIAN_POINT('Ctrl Pts',(88.2656759268388,-1.40176797156805,3.4497255103927));
#17069=CARTESIAN_POINT('Ctrl Pts',(88.2511212284633,-1.12213498214866,3.55625617283491));
#17070=CARTESIAN_POINT('Ctrl Pts',(88.2408891904004,-0.912555742871995,
3.61571432820128));
#17071=CARTESIAN_POINT('Ctrl Pts',(88.2238293571705,-0.568595911857687,
3.68146547383455));
#17072=CARTESIAN_POINT('Ctrl Pts',(88.2172465474274,-0.436979283891042,
3.69939649323452));
#17073=CARTESIAN_POINT('Ctrl Pts',(88.2075808615456,-0.248623401737625,
3.71486459231851));
#17074=CARTESIAN_POINT('Ctrl Pts',(88.2046686769021,-0.192458939123812,
3.71819736783688));
#17075=CARTESIAN_POINT('Ctrl Pts',(88.199410567924,-0.0922777503102582,
3.72186617905728));
#17076=CARTESIAN_POINT('Ctrl Pts',(88.1970800235928,-0.0482894160077024,
3.72269673117071));
#17077=CARTESIAN_POINT('Ctrl Pts',(88.1920512038369,0.045675523318885,3.72280521298625));
#17078=CARTESIAN_POINT('Ctrl Pts',(88.1893465157492,0.0956432750413966,
3.72185665290953));
#17079=CARTESIAN_POINT('Ctrl Pts',(88.1815489591566,0.238010934682628,3.71628521545284));
#17080=CARTESIAN_POINT('Ctrl Pts',(88.176384868378,0.330273709073209,3.70922394906707));
#17081=CARTESIAN_POINT('Ctrl Pts',(88.1639138913763,0.548452594274935,3.68432105785041));
#17082=CARTESIAN_POINT('Ctrl Pts',(88.1565342835466,0.673903304284392,3.66345089389269));
#17083=CARTESIAN_POINT('Ctrl Pts',(88.1340041738482,1.04870188561478,3.58119434181881));
#17084=CARTESIAN_POINT('Ctrl Pts',(88.1186174207522,1.29301327702992,3.50040750138304));
#17085=CARTESIAN_POINT('Ctrl Pts',(88.1016638876949,1.56732914839386,3.37702458832808));
#17086=CARTESIAN_POINT('Ctrl Pts',(88.0992061516287,1.6072594166623,3.35820386966895));
#17087=CARTESIAN_POINT('Ctrl Pts',(88.0953357535915,1.67058093034058,3.32696968179059));
#17088=CARTESIAN_POINT('Ctrl Pts',(88.0938988420199,1.69419011058612,3.31500948513039));
#17089=CARTESIAN_POINT('Ctrl Pts',(88.0910195852989,1.74175334161597,3.29027349926186));
#17090=CARTESIAN_POINT('Ctrl Pts',(88.0895780154058,1.76569904482905,3.27748552623805));
#17091=CARTESIAN_POINT('Ctrl Pts',(88.0856528786868,1.83117049553585,3.24159529216389));
#17092=CARTESIAN_POINT('Ctrl Pts',(88.0831995069761,1.87239824285088,3.21795752505246));
#17093=CARTESIAN_POINT('Ctrl Pts',(88.0776083441257,1.96664147456081,3.1614988693436));
#17094=CARTESIAN_POINT('Ctrl Pts',(88.0744965632663,2.01930816704048,3.12812227162595));
#17095=CARTESIAN_POINT('Ctrl Pts',(88.0630262870208,2.21271865012908,2.99863036463961));
#17096=CARTESIAN_POINT('Ctrl Pts',(88.0549291977798,2.34765205649643,2.89420841495331));
#17097=CARTESIAN_POINT('Ctrl Pts',(88.0377001601113,2.61589411043876,2.65547737525317));
#17098=CARTESIAN_POINT('Ctrl Pts',(88.028568807245,2.74708094977458,2.5195239403281));
#17099=CARTESIAN_POINT('Ctrl Pts',(88.0155702728691,2.91106095697644,2.32148233649355));
#17100=CARTESIAN_POINT('Ctrl Pts',(88.0120599387767,2.95326512942192,2.26754944294188));
#17101=CARTESIAN_POINT('Ctrl Pts',(88.0061150077484,3.02108938131016,2.17576901294856));
#17102=CARTESIAN_POINT('Ctrl Pts',(88.0037123161503,3.04754367464437,2.13855772859567));
#17103=CARTESIAN_POINT('Ctrl Pts',(87.9988320383362,3.09932029104117,2.06281512274474));
#17104=CARTESIAN_POINT('Ctrl Pts',(87.996354380982,3.12462444610435,2.02428118411595));
#17105=CARTESIAN_POINT('Ctrl Pts',(87.9899960297971,3.18705429220077,1.92525051834178));
#17106=CARTESIAN_POINT('Ctrl Pts',(87.9860808997728,3.22317623772767,1.86414555231813));
#17107=CARTESIAN_POINT('Ctrl Pts',(87.9772832650764,3.29926413536385,1.72660291012258));
#17108=CARTESIAN_POINT('Ctrl Pts',(87.9723760921402,3.33836426558408,1.64973453094291));
#17109=CARTESIAN_POINT('Ctrl Pts',(87.9549803074499,3.46570829470571,1.37628047658505));
#17110=CARTESIAN_POINT('Ctrl Pts',(87.942157336948,3.53952885300576,1.1734596664509));
#17111=CARTESIAN_POINT('Ctrl Pts',(87.9216902084876,3.62985705751071,0.837058930014744));
#17112=CARTESIAN_POINT('Ctrl Pts',(87.9139664269932,3.65742642669966,0.706942086733032));
#17113=CARTESIAN_POINT('Ctrl Pts',(87.9043972570307,3.68385937722709,0.538046536616738));
#17114=CARTESIAN_POINT('Ctrl Pts',(87.902292364192,3.68916405300237,0.500382653140881));
#17115=CARTESIAN_POINT('Ctrl Pts',(87.8988318747619,3.69704389965128,0.437467375902617));
#17116=CARTESIAN_POINT('Ctrl Pts',(87.8974603358787,3.69993965255739,0.412259630929676));
#17117=CARTESIAN_POINT('Ctrl Pts',(87.894543387535,3.70560890170458,0.358022895718634));
#17118=CARTESIAN_POINT('Ctrl Pts',(87.8930021655089,3.70829945672817,0.328987799342598));
#17119=CARTESIAN_POINT('Ctrl Pts',(87.8884430686021,3.71532233034682,0.242100830870248));
#17120=CARTESIAN_POINT('Ctrl Pts',(87.8854736056124,3.7186440205103,0.184174220970671));
#17121=CARTESIAN_POINT('Ctrl Pts',(87.8783813440398,3.7234163658059,0.04346646875734));
#17122=CARTESIAN_POINT('Ctrl Pts',(87.8743089036718,3.72346249377927,-0.0393323360391734));
#17123=CARTESIAN_POINT('Ctrl Pts',(87.8594338464656,3.71342955085848,-0.345148125767257));
#17124=CARTESIAN_POINT('Ctrl Pts',(87.8489373271024,3.68606373355316,-0.567118576897356));
#17125=CARTESIAN_POINT('Ctrl Pts',(87.8318671626106,3.61230146911092,-0.908921748915311));
#17126=CARTESIAN_POINT('Ctrl Pts',(87.8255830158037,3.57934451740969,-1.0310916031993));
#17127=CARTESIAN_POINT('Ctrl Pts',(87.8162560037859,3.52297290911332,-1.20442749242116));
#17128=CARTESIAN_POINT('Ctrl Pts',(87.8133650614059,3.50451740311575,-1.25711616704649));
#17129=CARTESIAN_POINT('Ctrl Pts',(87.8081300932156,3.46942550441721,-1.35051328465182));
#17130=CARTESIAN_POINT('Ctrl Pts',(87.8058008998807,3.45323918607512,-1.3913800231793));
#17131=CARTESIAN_POINT('Ctrl Pts',(87.8007578667453,3.41700555888998,-1.47833199256914));
#17132=CARTESIAN_POINT('Ctrl Pts',(87.7980372373347,3.39674115727954,-1.52431678084574));
#17133=CARTESIAN_POINT('Ctrl Pts',(87.7901339249019,3.3358707390591,-1.65520057680586));
#17134=CARTESIAN_POINT('Ctrl Pts',(87.7848768879323,3.29297034447667,-1.73898440702014));
#17135=CARTESIAN_POINT('Ctrl Pts',(87.7721085617985,3.18309057773597,-1.93490093686167));
#17136=CARTESIAN_POINT('Ctrl Pts',(87.7645194008865,3.11329660446284,-2.04530865349794));
#17137=CARTESIAN_POINT('Ctrl Pts',(87.742275316538,2.89451261941406,-2.35417958411365));
#17138=CARTESIAN_POINT('Ctrl Pts',(87.727427835427,2.73130802937129,-2.54171772147356));
#17139=CARTESIAN_POINT('Ctrl Pts',(87.710858425892,2.51748346668256,-2.74284882152555));
#17140=CARTESIAN_POINT('Ctrl Pts',(87.7083187301591,2.48373106724228,-2.7734496590092));
#17141=CARTESIAN_POINT('Ctrl Pts',(87.7043517833256,2.42928162071707,-2.82102353998803));
#17142=CARTESIAN_POINT('Ctrl Pts',(87.7028982765776,2.40894942727238,-2.83840549476555));
#17143=CARTESIAN_POINT('Ctrl Pts',(87.7000184430961,2.36784956789811,-2.87278191386471));
#17144=CARTESIAN_POINT('Ctrl Pts',(87.6985922848782,2.34708198230921,-2.88977399725392));
#17145=CARTESIAN_POINT('Ctrl Pts',(87.6947615729383,2.2902434042844,-2.93526244844375));
#17146=CARTESIAN_POINT('Ctrl Pts',(87.6923848240721,2.25382450216796,-2.96331840399038));
#17147=CARTESIAN_POINT('Ctrl Pts',(87.682048678778,2.09094646545296,-3.08405403837996));
#17148=CARTESIAN_POINT('Ctrl Pts',(87.6744482297694,1.95921706191711,-3.16937257260822));
#17149=CARTESIAN_POINT('Ctrl Pts',(87.6536483815622,1.581797621996,-3.38126875073741));
#17150=CARTESIAN_POINT('Ctrl Pts',(87.6405887357926,1.32684080338732,-3.48920426914433));
#17151=CARTESIAN_POINT('Ctrl Pts',(87.6233094273196,1.00041065447841,-3.5863931607547));
#17152=CARTESIAN_POINT('Ctrl Pts',(87.6199891560409,0.938054963181408,-3.60320546775309));
#17153=CARTESIAN_POINT('Ctrl Pts',(87.6142932199103,0.831997314829299,-3.62886104627075));
#17154=CARTESIAN_POINT('Ctrl Pts',(87.6119444459019,0.788515631628333,-3.63855670555856));
#17155=CARTESIAN_POINT('Ctrl Pts',(87.607073142924,0.69892880567694,-3.65685176832089));
#17156=CARTESIAN_POINT('Ctrl Pts',(87.6045484166771,0.652814335803341,-3.66536485286278));
#17157=CARTESIAN_POINT('Ctrl Pts',(87.597896535097,0.532206848534663,-3.6852817362447));
#17158=CARTESIAN_POINT('Ctrl Pts',(87.5937282719487,0.457509300951298,-3.69529833019803));
#17159=CARTESIAN_POINT('Ctrl Pts',(87.5842276491347,0.289230056115743,-3.71268332713183));
#17160=CARTESIAN_POINT('Ctrl Pts',(87.5788635215976,0.195571555858999,-3.71879301261899));
#17161=CARTESIAN_POINT('Ctrl Pts',(87.557741181702,-0.168912399694604,-3.72876240828649));
#17162=CARTESIAN_POINT('Ctrl Pts',(87.5414564413288,-0.439592765959358,
-3.70660867077501));
#17163=CARTESIAN_POINT('Ctrl Pts',(87.5216158054898,-0.777480969252871,
-3.6413967255353));
#17164=CARTESIAN_POINT('Ctrl Pts',(87.5174458439575,-0.849073018769935,
-3.62537212307217));
#17165=CARTESIAN_POINT('Ctrl Pts',(87.5115620788491,-0.951670457834807,
-3.59920118576324));
#17166=CARTESIAN_POINT('Ctrl Pts',(87.5097731145124,-0.983086560379654,
-3.59074738684396));
#17167=CARTESIAN_POINT('Ctrl Pts',(87.5066537677753,-1.03834604736253,-3.57509790453704));
#17168=CARTESIAN_POINT('Ctrl Pts',(87.5053147691838,-1.06223405641105,-3.56807320961385));
#17169=CARTESIAN_POINT('Ctrl Pts',(87.5022648064355,-1.11703208582513,-3.55135973168301));
#17170=CARTESIAN_POINT('Ctrl Pts',(87.5005627019815,-1.14788877774059,-3.54150647594772));
#17171=CARTESIAN_POINT('Ctrl Pts',(87.4948237603667,-1.25265933217468,-3.50653755900257));
#17172=CARTESIAN_POINT('Ctrl Pts',(87.4908800666779,-1.32591359060185,-3.47949933928717));
#17173=CARTESIAN_POINT('Ctrl Pts',(87.480464866776,-1.52042650957529,-3.4006682641765));
#17174=CARTESIAN_POINT('Ctrl Pts',(87.4741274708399,-1.63987558698074,-3.34470515313688));
#17175=CARTESIAN_POINT('Ctrl Pts',(87.4561239794847,-1.97099806715439,-3.16755869329075));
#17176=CARTESIAN_POINT('Ctrl Pts',(87.4445062287557,-2.17406275107045,-3.03178217094962));
#17177=CARTESIAN_POINT('Ctrl Pts',(87.4287368014681,-2.41507099362414,-2.83389210615855));
#17178=CARTESIAN_POINT('Ctrl Pts',(87.4252420769192,-2.46654333218421,-2.78920699130686));
#17179=CARTESIAN_POINT('Ctrl Pts',(87.4195528302774,-2.54700536977767,-2.71538509276096));
#17180=CARTESIAN_POINT('Ctrl Pts',(87.4173943726057,-2.5767904971737,-2.6871366014865));
#17181=CARTESIAN_POINT('Ctrl Pts',(87.4128111605039,-2.63843961168021,-2.62670034812941));
#17182=CARTESIAN_POINT('Ctrl Pts',(87.4103823029705,-2.67019538195899,-2.59441220387761));
#17183=CARTESIAN_POINT('Ctrl Pts',(87.4043335722367,-2.7469975207394,-2.5134185033366));
#17184=CARTESIAN_POINT('Ctrl Pts',(87.4006859037732,-2.79134481003505,-2.4640741360887));
#17185=CARTESIAN_POINT('Ctrl Pts',(87.3871474939668,-2.94877758204568,-2.27919501561617));
#17186=CARTESIAN_POINT('Ctrl Pts',(87.3769533275565,-3.0534937830724,-2.13686296876134));
#17187=CARTESIAN_POINT('Ctrl Pts',(87.3515944429072,-3.28406238274875,-1.77172740916098));
#17188=CARTESIAN_POINT('Ctrl Pts',(87.3362863661774,-3.39783466331522,-1.54233940597438));
#17189=CARTESIAN_POINT('Ctrl Pts',(87.3193882640276,-3.50275494364628,-1.26156341839448));
#17190=CARTESIAN_POINT('Ctrl Pts',(87.3169182809703,-3.51753611034684,-1.21974362212606));
#17191=CARTESIAN_POINT('Ctrl Pts',(87.3130334363718,-3.5399522561828,-1.15252253360953));
#17192=CARTESIAN_POINT('Ctrl Pts',(87.3115940290524,-3.54806898962337,-1.12728732701567));
#17193=CARTESIAN_POINT('Ctrl Pts',(87.3087148198242,-3.56393618913984,-1.07608575332492));
#17194=CARTESIAN_POINT('Ctrl Pts',(87.3072756988858,-3.57167403712233,-1.05011731227512));
#17195=CARTESIAN_POINT('Ctrl Pts',(87.303365493146,-3.59213163717905,-0.978617651118007));
#17196=CARTESIAN_POINT('Ctrl Pts',(87.3009242219604,-3.60426909844324,-0.932923821940991));
#17197=CARTESIAN_POINT('Ctrl Pts',(87.2953666510638,-3.63028112174045,-0.826896364906126));
#17198=CARTESIAN_POINT('Ctrl Pts',(87.2922759131574,-3.64352793565999,-0.766422482730354));
#17199=CARTESIAN_POINT('Ctrl Pts',(87.2775961180349,-3.69997106573645,-0.474045101324363));
#17200=CARTESIAN_POINT('Ctrl Pts',(87.2665385515448,-3.72256915154514,-0.238720185061259));
#17201=CARTESIAN_POINT('Ctrl Pts',(87.2551011079057,-3.72274891890995,-0.00283712086446175));
#17202=CARTESIAN_POINT('Ctrl Pts',(87.2551009553192,-3.72274892130689,-0.00283397395788376));
#17203=CARTESIAN_POINT('Ctrl Pts',(87.2481690907567,-3.72285775161648,0.140127084840354));
#17204=CARTESIAN_POINT('Ctrl Pts',(87.2411206974449,-3.71473158564361,0.282969156473876));
#17205=CARTESIAN_POINT('Ctrl Pts',(87.2314476587175,-3.69306159874725,0.471551346865502));
#17206=CARTESIAN_POINT('Ctrl Pts',(87.2290352459888,-3.68683178562366,0.518011379072727));
#17207=CARTESIAN_POINT('Ctrl Pts',(87.2241973229379,-3.67273551875958,0.609924749068469));
#17208=CARTESIAN_POINT('Ctrl Pts',(87.2217730790791,-3.66489822330142,0.655374058299254));
#17209=CARTESIAN_POINT('Ctrl Pts',(87.2168980386484,-3.64763040186785,0.745481248027248));
#17210=CARTESIAN_POINT('Ctrl Pts',(87.2144482110008,-3.63821892122694,0.790134591914953));
#17211=CARTESIAN_POINT('Ctrl Pts',(87.2082648874663,-3.61266472449791,0.901217850442107));
#17212=CARTESIAN_POINT('Ctrl Pts',(87.2045007518601,-3.5955090541113,0.967395391167315));
#17213=CARTESIAN_POINT('Ctrl Pts',(87.18242114745,-3.48580302326893,1.34720690893251));
#17214=CARTESIAN_POINT('Ctrl Pts',(87.1628606429618,-3.35407526029626,1.64800092110445));
#17215=CARTESIAN_POINT('Ctrl Pts',(87.1390495266081,-3.14347056822796,1.99595423378076));
#17216=CARTESIAN_POINT('Ctrl Pts',(87.1344169459925,-3.09994577583506,2.06290519015491));
#17217=CARTESIAN_POINT('Ctrl Pts',(87.1266436286505,-3.021947026892,2.1748346923464));
#17218=CARTESIAN_POINT('Ctrl Pts',(87.1234623852895,-2.98853786527519,2.2205206253762));
#17219=CARTESIAN_POINT('Ctrl Pts',(87.1187467974954,-2.93651370615651,2.28835964007137));
#17220=CARTESIAN_POINT('Ctrl Pts',(87.1171685721622,-2.91866197932996,2.31108523107678));
#17221=CARTESIAN_POINT('Ctrl Pts',(87.1142492723602,-2.8847677687392,2.35321399776764));
#17222=CARTESIAN_POINT('Ctrl Pts',(87.1129043839747,-2.86879029564076,2.3726658958337));
#17223=CARTESIAN_POINT('Ctrl Pts',(87.1095430509435,-2.8279713376069,2.4213460950567));
#17224=CARTESIAN_POINT('Ctrl Pts',(87.1075437435319,-2.80287255399562,2.45035598743111));
#17225=CARTESIAN_POINT('Ctrl Pts',(87.1016745714368,-2.7269375600657,2.53543008319701));
#17226=CARTESIAN_POINT('Ctrl Pts',(87.0978789969963,-2.67484318990745,2.59032912354232));
#17227=CARTESIAN_POINT('Ctrl Pts',(87.0941439883772,-2.62111999291044,2.64359557142638));
#17228=CARTESIAN_POINT('Ctrl Pts',(86.8469367975669,-2.62112000772923,2.64359555673358));
#17229=CARTESIAN_POINT('Ctrl Pts',(86.8479364796116,-2.63422751735572,2.6305994856644));
#17230=CARTESIAN_POINT('Ctrl Pts',(86.8489402927088,-2.64723833041324,2.61750597024224));
#17231=CARTESIAN_POINT('Ctrl Pts',(86.8545857674141,-2.71956531200265,2.54362833282821));
#17232=CARTESIAN_POINT('Ctrl Pts',(86.8593090595828,-2.77688156213494,2.48092882258983));
#17233=CARTESIAN_POINT('Ctrl Pts',(86.8810117078852,-3.02607124839538,2.18887180157179));
#17234=CARTESIAN_POINT('Ctrl Pts',(86.898909857695,-3.19201871212538,1.93887702829356));
#17235=CARTESIAN_POINT('Ctrl Pts',(86.9209505092802,-3.36122010782939,1.60222574810387));
#17236=CARTESIAN_POINT('Ctrl Pts',(86.925463694497,-3.39399089429002,1.5315857253983));
#17237=CARTESIAN_POINT('Ctrl Pts',(86.9330629058012,-3.44633387571132,1.40880914677604));
#17238=CARTESIAN_POINT('Ctrl Pts',(86.9361872946315,-3.4669959917596,1.35716609388758));
#17239=CARTESIAN_POINT('Ctrl Pts',(86.9408372646071,-3.49656103651619,1.27818350914106));
#17240=CARTESIAN_POINT('Ctrl Pts',(86.9424050266554,-3.50631672641429,1.25117356252425));
#17241=CARTESIAN_POINT('Ctrl Pts',(86.9453171800885,-3.52405761641445,1.20021766626114));
#17242=CARTESIAN_POINT('Ctrl Pts',(86.9466651110412,-3.5321133678115,1.17629915499785));
#17243=CARTESIAN_POINT('Ctrl Pts',(86.9500513466499,-3.5519303731355,1.11542029135123));
#17244=CARTESIAN_POINT('Ctrl Pts',(86.9520719292542,-3.56335870890518,1.07835371793144));
#17245=CARTESIAN_POINT('Ctrl Pts',(86.96161878224,-3.61526387232496,0.900160204006547));
#17246=CARTESIAN_POINT('Ctrl Pts',(86.968800275248,-3.64795117390932,0.756888770379204));
#17247=CARTESIAN_POINT('Ctrl Pts',(86.9857386298002,-3.70566792992219,0.410608304780262));
#17248=CARTESIAN_POINT('Ctrl Pts',(86.9953903594235,-3.72261047931251,0.20674836417901));
#17249=CARTESIAN_POINT('Ctrl Pts',(87.0111802735306,-3.72282939123067,-0.11566265239382));
#17250=CARTESIAN_POINT('Ctrl Pts',(87.0170716576226,-3.71728119422797,-0.233781980183838));
#17251=CARTESIAN_POINT('Ctrl Pts',(87.0259674608812,-3.70088901968681,-0.406650390857667));
#17252=CARTESIAN_POINT('Ctrl Pts',(87.0288432021793,-3.69441970680641,-0.461743105891317));
#17253=CARTESIAN_POINT('Ctrl Pts',(87.034059677121,-3.68063605131306,-0.560097198287279));
#17254=CARTESIAN_POINT('Ctrl Pts',(87.0363859344194,-3.67378319037585,-0.603413181308806));
#17255=CARTESIAN_POINT('Ctrl Pts',(87.041475400076,-3.65728775048501,-0.696941379411489));
#17256=CARTESIAN_POINT('Ctrl Pts',(87.0442465761122,-3.64737280347217,-0.74709588359248));
#17257=CARTESIAN_POINT('Ctrl Pts',(87.052493830743,-3.61516685725108,-0.894034908728921));
#17258=CARTESIAN_POINT('Ctrl Pts',(87.0580549112132,-3.59003352505528,-0.990144780847397));
#17259=CARTESIAN_POINT('Ctrl Pts',(87.0718264483764,-3.51961544840658,-1.2212371022127));
#17260=CARTESIAN_POINT('Ctrl Pts',(87.0801337058674,-3.47037460852577,-1.35484618256512));
#17261=CARTESIAN_POINT('Ctrl Pts',(87.1023570125416,-3.31986942264083,-1.70074657191134));
#17262=CARTESIAN_POINT('Ctrl Pts',(87.1163753574549,-3.20593745829391,-1.90684223360547));
#17263=CARTESIAN_POINT('Ctrl Pts',(87.1319390803758,-3.04972998165191,-2.13536042330805));
#17264=CARTESIAN_POINT('Ctrl Pts',(87.1342631556041,-3.0255445483069,-2.1694924689364));
#17265=CARTESIAN_POINT('Ctrl Pts',(87.1378367368629,-2.9869042542877,-2.22212080645775));
#17266=CARTESIAN_POINT('Ctrl Pts',(87.1391098227967,-2.97284164384179,-2.24089949017644));
#17267=CARTESIAN_POINT('Ctrl Pts',(87.1418131221603,-2.94231347999386,-2.28087245316507));
#17268=CARTESIAN_POINT('Ctrl Pts',(87.1432395204213,-2.92579425549943,-2.30202428804485));
#17269=CARTESIAN_POINT('Ctrl Pts',(87.1470716623311,-2.88034952011591,-2.35893392876347));
#17270=CARTESIAN_POINT('Ctrl Pts',(87.1494495660655,-2.85098707137756,-2.39433826255021));
#17271=CARTESIAN_POINT('Ctrl Pts',(87.1597971322618,-2.71853978565936,-2.5481468719549));
#17272=CARTESIAN_POINT('Ctrl Pts',(87.1674069396115,-2.60867457506647,-2.66051416042603));
#17273=CARTESIAN_POINT('Ctrl Pts',(87.1881988675785,-2.2872360604958,-2.95015530535578));
#17274=CARTESIAN_POINT('Ctrl Pts',(87.2012426963686,-2.06259001495656,-3.1113627893878));
#17275=CARTESIAN_POINT('Ctrl Pts',(87.2185055481398,-1.76585917063264,-3.2779238780769));
#17276=CARTESIAN_POINT('Ctrl Pts',(87.2218281542193,-1.70869613796958,-3.30808108175837));
#17277=CARTESIAN_POINT('Ctrl Pts',(87.2275268431535,-1.61084408063918,-3.35649133298813));
#17278=CARTESIAN_POINT('Ctrl Pts',(87.2298759696225,-1.57055866677803,-3.3755292874633));
#17279=CARTESIAN_POINT('Ctrl Pts',(87.2347469053028,-1.48720569969636,-3.41310479744019));
#17280=CARTESIAN_POINT('Ctrl Pts',(87.2372708889242,-1.44411034448974,-3.43156089781793));
#17281=CARTESIAN_POINT('Ctrl Pts',(87.2439181074332,-1.33092802690625,-3.47752292530341));
#17282=CARTESIAN_POINT('Ctrl Pts',(87.2480823406078,-1.26033736765293,-3.50372426654168));
#17283=CARTESIAN_POINT('Ctrl Pts',(87.2575716186588,-1.10020638506853,-3.55769507396356));
#17284=CARTESIAN_POINT('Ctrl Pts',(87.2629283091363,-1.01031528612291,-3.58425857731229));
#17285=CARTESIAN_POINT('Ctrl Pts',(87.283977320029,-0.658195193161684,-3.67401356369224));
#17286=CARTESIAN_POINT('Ctrl Pts',(87.3001917683876,-0.390421990427456,
-3.7120286053518));
#17287=CARTESIAN_POINT('Ctrl Pts',(87.3200343578389,-0.0466224385883072,
-3.72319984360815));
#17288=CARTESIAN_POINT('Ctrl Pts',(87.3242618314156,0.0277165204521502,
-3.72338875439068));
#17289=CARTESIAN_POINT('Ctrl Pts',(87.3302099504557,0.134690041883209,-3.72045623482529));
#17290=CARTESIAN_POINT('Ctrl Pts',(87.3320078983521,0.167352699612359,-3.719130170331));
#17291=CARTESIAN_POINT('Ctrl Pts',(87.3351364793589,0.224861542560495,-3.71603619417132));
#17292=CARTESIAN_POINT('Ctrl Pts',(87.3364759358832,0.249713815552624,-3.71444892299767));
#17293=CARTESIAN_POINT('Ctrl Pts',(87.339518691028,0.306702147011486,-3.71023459424388));
#17294=CARTESIAN_POINT('Ctrl Pts',(87.3412133363148,0.338822743015615,-3.70743931023352));
#17295=CARTESIAN_POINT('Ctrl Pts',(87.3468914138761,0.44753004302278,-3.69655445479987));
#17296=CARTESIAN_POINT('Ctrl Pts',(87.3507843729499,0.523904181608227,-3.68650563295299));
#17297=CARTESIAN_POINT('Ctrl Pts',(87.3610051965339,0.727037625838374,-3.65333746757463));
#17298=CARTESIAN_POINT('Ctrl Pts',(87.3672049614466,0.853002435697202,-3.6259961623754));
#17299=CARTESIAN_POINT('Ctrl Pts',(87.3853294290354,1.21768742178242,-3.52677865571833));
#17300=CARTESIAN_POINT('Ctrl Pts',(87.3971897218197,1.45088336110006,-3.4374202971593));
#17301=CARTESIAN_POINT('Ctrl Pts',(87.4132164432478,1.73387672085105,-3.29501475000028));
#17302=CARTESIAN_POINT('Ctrl Pts',(87.4166890444941,1.79350651972013,-3.26294105661915));
#17303=CARTESIAN_POINT('Ctrl Pts',(87.422352220358,1.88777192734261,-3.20887267674082));
#17304=CARTESIAN_POINT('Ctrl Pts',(87.4245073942538,1.92297727551404,-3.1878997678052));
#17305=CARTESIAN_POINT('Ctrl Pts',(87.4290916599385,1.99640811883289,-3.14249576476093));
#17306=CARTESIAN_POINT('Ctrl Pts',(87.4315250083056,2.03454744586019,-3.11793865493081));
#17307=CARTESIAN_POINT('Ctrl Pts',(87.437602829122,2.12769925292349,-3.05552320442431));
#17308=CARTESIAN_POINT('Ctrl Pts',(87.4412757065344,2.18215837471395,-3.01687093218046));
#17309=CARTESIAN_POINT('Ctrl Pts',(87.4550181335572,2.37917856232542,-2.86890962359895));
#17310=CARTESIAN_POINT('Ctrl Pts',(87.4654029242124,2.51480052860258,-2.75079975746461));
#17311=CARTESIAN_POINT('Ctrl Pts',(87.4906169203798,2.8171903884149,-2.44633723384258));
#17312=CARTESIAN_POINT('Ctrl Pts',(87.5055598564812,2.97478281745828,-2.25206625253012));
#17313=CARTESIAN_POINT('Ctrl Pts',(87.5221979204017,3.13662762464533,-2.0056140061411));
#17314=CARTESIAN_POINT('Ctrl Pts',(87.524723416456,3.16080578772355,-1.96728938569164));
#17315=CARTESIAN_POINT('Ctrl Pts',(87.5286736405184,3.19811019125227,-1.90569451409617));
#17316=CARTESIAN_POINT('Ctrl Pts',(87.5301242732166,3.21169549468296,-1.88270882490503));
#17317=CARTESIAN_POINT('Ctrl Pts',(87.5330038715898,3.23846143424558,-1.83628914170717));
#17318=CARTESIAN_POINT('Ctrl Pts',(87.5344325671078,3.25163783794852,-1.81285458058579));
#17319=CARTESIAN_POINT('Ctrl Pts',(87.5382787954765,3.28677510326585,-1.74874623300434));
#17320=CARTESIAN_POINT('Ctrl Pts',(87.540668136028,3.3082347498521,-1.7078018532505));
#17321=CARTESIAN_POINT('Ctrl Pts',(87.5511302798696,3.40012586061098,-1.52424054512313));
#17322=CARTESIAN_POINT('Ctrl Pts',(87.5588340105021,3.46214236139758,-1.3775860026505));
#17323=CARTESIAN_POINT('Ctrl Pts',(87.5795487335213,3.6043153584574,-0.970483077624764));
#17324=CARTESIAN_POINT('Ctrl Pts',(87.5924355060725,3.66559280489559,-0.704518797517292));
#17325=CARTESIAN_POINT('Ctrl Pts',(87.6095350419798,3.70492816148626,-0.369610038076758));
#17326=CARTESIAN_POINT('Ctrl Pts',(87.6128804713385,3.7108238037798,-0.304779135170445));
#17327=CARTESIAN_POINT('Ctrl Pts',(87.6186060037733,3.71789194415081,-0.195291847803361));
#17328=CARTESIAN_POINT('Ctrl Pts',(87.6209585039582,3.71996591358417,-0.1507076332699));
#17329=CARTESIAN_POINT('Ctrl Pts',(87.6258257272487,3.7225703017399,-0.0593624922091599));
#17330=CARTESIAN_POINT('Ctrl Pts',(87.6283424018644,3.72302220549708,-0.0126074339512018));
#17331=CARTESIAN_POINT('Ctrl Pts',(87.6349442261392,3.72190919782321,0.108745468813719));
#17332=CARTESIAN_POINT('Ctrl Pts',(87.6390693189485,3.71898252928336,0.183307218808084));
#17333=CARTESIAN_POINT('Ctrl Pts',(87.6549751713529,3.69936344359356,0.466015731787855));
#17334=CARTESIAN_POINT('Ctrl Pts',(87.6671787102698,3.6674134402773,0.672697643241746));
#17335=CARTESIAN_POINT('Ctrl Pts',(87.6916779648745,3.56978379992552,1.07614544228474));
#17336=CARTESIAN_POINT('Ctrl Pts',(87.7039236488903,3.50465867448407,1.27232955497797));
#17337=CARTESIAN_POINT('Ctrl Pts',(87.7180507508391,3.40623009844991,1.50280464348935));
#17338=CARTESIAN_POINT('Ctrl Pts',(87.7205147400571,3.38812758013524,1.54318408365587));
#17339=CARTESIAN_POINT('Ctrl Pts',(87.7243925271119,3.35804459129501,1.60720427936572));
#17340=CARTESIAN_POINT('Ctrl Pts',(87.7258307251976,3.3465245237232,1.63105572939414));
#17341=CARTESIAN_POINT('Ctrl Pts',(87.7287099614352,3.32269575581642,1.67907591623779));
#17342=CARTESIAN_POINT('Ctrl Pts',(87.7301502727207,3.31037562820098,1.70323700841885));
#17343=CARTESIAN_POINT('Ctrl Pts',(87.7340677689931,3.27580365047861,1.76924390068868));
#17344=CARTESIAN_POINT('Ctrl Pts',(87.7365149537306,3.25301447287883,1.81080389995596));
#17345=CARTESIAN_POINT('Ctrl Pts',(87.7420889398034,3.19853845215192,1.9058009603829));
#17346=CARTESIAN_POINT('Ctrl Pts',(87.74518996026,3.16629500438848,1.95890329002019));
#17347=CARTESIAN_POINT('Ctrl Pts',(87.7565881115289,3.04136459826023,2.15350290523736));
#17348=CARTESIAN_POINT('Ctrl Pts',(87.7646270543949,2.9403959173098,2.28944312515968));
#17349=CARTESIAN_POINT('Ctrl Pts',(87.7818704548197,2.70692523298511,2.56274003902158));
#17350=CARTESIAN_POINT('Ctrl Pts',(87.7910765237114,2.57241523266802,2.69773109042674));
#17351=CARTESIAN_POINT('Ctrl Pts',(87.8041592762334,2.37624893711966,2.86653155596696));
#17352=CARTESIAN_POINT('Ctrl Pts',(87.8076717498739,2.32309130700325,2.90977803577831));
#17353=CARTESIAN_POINT('Ctrl Pts',(87.8136191764263,2.23257130861604,2.97935862146883));
#17354=CARTESIAN_POINT('Ctrl Pts',(87.8160221582096,2.19586222813033,3.00651646896838));
#17355=CARTESIAN_POINT('Ctrl Pts',(87.8209021046976,2.12111676162474,3.05971488463199));
#17356=CARTESIAN_POINT('Ctrl Pts',(87.8233791210617,2.08307778739298,3.08573786443446));
#17357=CARTESIAN_POINT('Ctrl Pts',(87.8297337741589,1.98530165133014,3.1499959130774));
#17358=CARTESIAN_POINT('Ctrl Pts',(87.8336457693517,1.9249388043878,3.18724121779741));
#17359=CARTESIAN_POINT('Ctrl Pts',(87.842434838972,1.78899196916851,3.26585261383944));
#17360=CARTESIAN_POINT('Ctrl Pts',(87.8473365025625,1.71296246437522,3.30636412224572));
#17361=CARTESIAN_POINT('Ctrl Pts',(87.8646942012464,1.44256292290409,3.43861261495007));
#17362=CARTESIAN_POINT('Ctrl Pts',(87.8774829307486,1.24172047149406,3.51612925744599));
#17363=CARTESIAN_POINT('Ctrl Pts',(87.8979093327466,0.907853699762734,3.61279422665573));
#17364=CARTESIAN_POINT('Ctrl Pts',(87.9056244925012,0.778483215665688,3.64286282434161));
#17365=CARTESIAN_POINT('Ctrl Pts',(87.9152138243616,0.609880139217438,3.67265498286814));
#17366=CARTESIAN_POINT('Ctrl Pts',(87.9173446773599,0.571882387746015,3.67876326663993));
#17367=CARTESIAN_POINT('Ctrl Pts',(87.9208210960351,0.50886551351341,3.68789343575293));
#17368=CARTESIAN_POINT('Ctrl Pts',(87.922183470224,0.483898752501437,3.69125239372366));
#17369=CARTESIAN_POINT('Ctrl Pts',(87.9250754732839,0.430275040529855,3.69791331365455));
#17370=CARTESIAN_POINT('Ctrl Pts',(87.9266010774839,0.40161068795367,3.70113610190029));
#17371=CARTESIAN_POINT('Ctrl Pts',(87.9310573710264,0.316896596990574,3.70966487880494));
#17372=CARTESIAN_POINT('Ctrl Pts',(87.9339428654183,0.260758826245031,3.71403317356625));
#17373=CARTESIAN_POINT('Ctrl Pts',(87.9407811663344,0.125423756418805,3.72148020688869));
#17374=CARTESIAN_POINT('Ctrl Pts',(87.9446883223599,0.0461841225284874,
3.72330688661744));
#17375=CARTESIAN_POINT('Ctrl Pts',(87.9560573757369,-0.187217556062976,
3.72123428886023));
#17376=CARTESIAN_POINT('Ctrl Pts',(87.9633811875971,-0.341147620794925,
3.71029048216468));
#17377=CARTESIAN_POINT('Ctrl Pts',(87.9791688657614,-0.666756416640207,
3.66670120513344));
#17378=CARTESIAN_POINT('Ctrl Pts',(87.9876415994009,-0.837705950818567,
3.63146032299565));
#17379=CARTESIAN_POINT('Ctrl Pts',(87.9998951845842,-1.07097413608624,3.56602012381194));
#17380=CARTESIAN_POINT('Ctrl Pts',(88.0033801533852,-1.13588333395329,3.54587837599045));
#17381=CARTESIAN_POINT('Ctrl Pts',(88.0090578889367,-1.23902946790542,3.51074862841467));
#17382=CARTESIAN_POINT('Ctrl Pts',(88.0112148840295,-1.2776340565427,3.49688447019403));
#17383=CARTESIAN_POINT('Ctrl Pts',(88.0157985028227,-1.35839172687864,3.46636597964745));
#17384=CARTESIAN_POINT('Ctrl Pts',(88.0182292967322,-1.40048534972577,3.44957413767248));
#17385=CARTESIAN_POINT('Ctrl Pts',(88.0242906514219,-1.5035908334653,3.40624541108988));
#17386=CARTESIAN_POINT('Ctrl Pts',(88.0279492723866,-1.56421615394356,3.37883415651275));
#17387=CARTESIAN_POINT('Ctrl Pts',(88.0415759974627,-1.78410681576667,3.27222578103474));
#17388=CARTESIAN_POINT('Ctrl Pts',(88.0518526138274,-1.93835925768443,3.18327666591451));
#17389=CARTESIAN_POINT('Ctrl Pts',(88.0758998126273,-2.27747090228849,2.95391618451089));
#17390=CARTESIAN_POINT('Ctrl Pts',(88.0897456316995,-2.45673161419878,2.80658633874833));
#17391=CARTESIAN_POINT('Ctrl Pts',(88.1029424526342,-2.62112000712061,2.64359555733703));
#17392=CARTESIAN_POINT('Origin',(80.1322559480305,0.,0.));
#17393=CARTESIAN_POINT('',(89.5984125828405,-2.62112000708803,2.64359555736933));
#17394=CARTESIAN_POINT('',(89.3502471949048,-2.62112000711957,2.64359555733806));
#17395=CARTESIAN_POINT('',(80.1322559480305,-2.62112000711956,2.64359555733806));
#17396=CARTESIAN_POINT('Ctrl Pts',(89.5984125828405,-2.62112000708803,2.64359555736933));
#17397=CARTESIAN_POINT('Ctrl Pts',(89.5983783641608,-2.62062322410473,2.64408811675992));
#17398=CARTESIAN_POINT('Ctrl Pts',(89.5983441417931,-2.62012629914963,2.64458053922071));
#17399=CARTESIAN_POINT('Ctrl Pts',(89.5940672226702,-2.55801239983286,2.70609694998344));
#17400=CARTESIAN_POINT('Ctrl Pts',(89.5897715287192,-2.49428457319044,2.76494692445715));
#17401=CARTESIAN_POINT('Ctrl Pts',(89.5818024515098,-2.37457448280402,2.86798494521362));
#17402=CARTESIAN_POINT('Ctrl Pts',(89.5781567756307,-2.31926640413608,2.91289274651102));
#17403=CARTESIAN_POINT('Ctrl Pts',(89.5720486682154,-2.22605659882886,2.98423687113263));
#17404=CARTESIAN_POINT('Ctrl Pts',(89.5696221294293,-2.18888958018596,3.01160419756669));
#17405=CARTESIAN_POINT('Ctrl Pts',(89.564744420832,-2.11398378151335,3.06464064227982));
#17406=CARTESIAN_POINT('Ctrl Pts',(89.5622942623307,-2.07626268607018,3.09032080947083));
#17407=CARTESIAN_POINT('Ctrl Pts',(89.5561154233189,-1.98096357064162,3.15266704013429));
#17408=CARTESIAN_POINT('Ctrl Pts',(89.5523562289654,-1.92283289339163,3.18845401018746));
#17409=CARTESIAN_POINT('Ctrl Pts',(89.5387248150602,-1.71159530661769,3.31062003856433));
#17410=CARTESIAN_POINT('Ctrl Pts',(89.5285562197113,-1.55341103921713,3.38772288606427));
#17411=CARTESIAN_POINT('Ctrl Pts',(89.5042347038918,-1.16972155402383,3.54220355641211));
#17412=CARTESIAN_POINT('Ctrl Pts',(89.4899833755887,-0.941045374096862,
3.60969434419777));
#17413=CARTESIAN_POINT('Ctrl Pts',(89.4733109962255,-0.653567184568792,
3.665342291024));
#17414=CARTESIAN_POINT('Ctrl Pts',(89.4702253776539,-0.599417279623072,
3.67458619475536));
#17415=CARTESIAN_POINT('Ctrl Pts',(89.4656234302423,-0.516859172122235,
3.68680593828053));
#17416=CARTESIAN_POINT('Ctrl Pts',(89.4640658087192,-0.488590273830709,
3.69065862383654));
#17417=CARTESIAN_POINT('Ctrl Pts',(89.4611700664737,-0.435353971747939,
3.69729162813848));
#17418=CARTESIAN_POINT('Ctrl Pts',(89.4598284813527,-0.410398360110441,
3.70014481674375));
#17419=CARTESIAN_POINT('Ctrl Pts',(89.456456987742,-0.346999767700094,3.70674391682602));
#17420=CARTESIAN_POINT('Ctrl Pts',(89.4544447785617,-0.308522879156999,
3.71014462828397));
#17421=CARTESIAN_POINT('Ctrl Pts',(89.4455349651245,-0.135760963104638,
3.72270755719113));
#17422=CARTESIAN_POINT('Ctrl Pts',(89.4389253008588,-0.00108147445861484,
3.72518283535709));
#17423=CARTESIAN_POINT('Ctrl Pts',(89.4220947337345,0.346743232374871,3.71270672055372));
#17424=CARTESIAN_POINT('Ctrl Pts',(89.4120381197272,0.558985311581401,3.6867273275733));
#17425=CARTESIAN_POINT('Ctrl Pts',(89.3974058109574,0.851795286390328,3.62500692511691));
#17426=CARTESIAN_POINT('Ctrl Pts',(89.3931568442392,0.935116938229867,3.6044119675721));
#17427=CARTESIAN_POINT('Ctrl Pts',(89.3852653390836,1.08561891704466,3.56164176340111));
#17428=CARTESIAN_POINT('Ctrl Pts',(89.381649922375,1.15302144112462,3.5403956330067));
#17429=CARTESIAN_POINT('Ctrl Pts',(89.3755879542324,1.26311629123043,3.50221488274077));
#17430=CARTESIAN_POINT('Ctrl Pts',(89.3731768517124,1.30617367567886,3.48638522468907));
#17431=CARTESIAN_POINT('Ctrl Pts',(89.3683282427091,1.39123173044083,3.45331754671148));
#17432=CARTESIAN_POINT('Ctrl Pts',(89.36589169485,1.43323141892593,3.43609884332223));
#17433=CARTESIAN_POINT('Ctrl Pts',(89.3597446531757,1.53728698918597,3.39119925772627));
#17434=CARTESIAN_POINT('Ctrl Pts',(89.356003766226,1.59891779859629,3.36258007367754));
#17435=CARTESIAN_POINT('Ctrl Pts',(89.3385012332598,1.87946910535744,3.22284471546164));
#17436=CARTESIAN_POINT('Ctrl Pts',(89.3240892785822,2.08781964671588,3.09194322582734));
#17437=CARTESIAN_POINT('Ctrl Pts',(89.3018288905159,2.38550101991659,2.86103045001828));
#17438=CARTESIAN_POINT('Ctrl Pts',(89.2940721916139,2.48492899756692,2.77511090781314));
#17439=CARTESIAN_POINT('Ctrl Pts',(89.2819941482718,2.63573790176689,2.63017358322949));
#17440=CARTESIAN_POINT('Ctrl Pts',(89.2775638755336,2.69016210078442,2.57448183728359));
#17441=CARTESIAN_POINT('Ctrl Pts',(89.2714489260246,2.76461953592262,2.49334864867993));
#17442=CARTESIAN_POINT('Ctrl Pts',(89.269675875928,2.78612688011295,2.46929257350742));
#17443=CARTESIAN_POINT('Ctrl Pts',(89.2665758784359,2.82364211182132,2.42621731722322));
#17444=CARTESIAN_POINT('Ctrl Pts',(89.2652406031047,2.83977606716401,2.40731327242714));
#17445=CARTESIAN_POINT('Ctrl Pts',(89.2621896989433,2.87657031098183,2.36331695699411));
#17446=CARTESIAN_POINT('Ctrl Pts',(89.2604831342135,2.89709311300202,2.33811364757034));
#17447=CARTESIAN_POINT('Ctrl Pts',(89.2549991535411,2.9627095556348,2.25534181007875));
#17448=CARTESIAN_POINT('Ctrl Pts',(89.2513004311705,3.00643963714966,2.19671038053934));
#17449=CARTESIAN_POINT('Ctrl Pts',(89.2341828314028,3.20405656256711,1.91478814402373));
#17450=CARTESIAN_POINT('Ctrl Pts',(89.2215597811034,3.33497924789401,1.67640183366802));
#17451=CARTESIAN_POINT('Ctrl Pts',(89.2037802820463,3.47483114918058,1.33911945690627));
#17452=CARTESIAN_POINT('Ctrl Pts',(89.1991494151813,3.5075135695305,1.2510154516963));
#17453=CARTESIAN_POINT('Ctrl Pts',(89.1906329048216,3.5603781639106,1.09007784498255));
#17454=CARTESIAN_POINT('Ctrl Pts',(89.1867820628437,3.58174196863675,1.01768654050678));
#17455=CARTESIAN_POINT('Ctrl Pts',(89.1804224464142,3.61281690981811,0.899238788898053));
#17456=CARTESIAN_POINT('Ctrl Pts',(89.1779559852729,3.6238811081814,0.853558362164017));
#17457=CARTESIAN_POINT('Ctrl Pts',(89.1730914913085,3.64377253339684,0.764059060087203));
#17458=CARTESIAN_POINT('Ctrl Pts',(89.1706964607138,3.65268128352727,0.720266431089842));
#17459=CARTESIAN_POINT('Ctrl Pts',(89.1647644245985,3.67258576521568,0.612527867379545));
#17460=CARTESIAN_POINT('Ctrl Pts',(89.1612013160963,3.68270194932705,0.548436175317296));
#17461=CARTESIAN_POINT('Ctrl Pts',(89.140610942521,3.7308000276898,0.181712396717437));
#17462=CARTESIAN_POINT('Ctrl Pts',(89.1225069996574,3.7331439834418,-0.124386153354806));
#17463=CARTESIAN_POINT('Ctrl Pts',(89.098915095069,3.68709889795588,-0.522912248360082));
#17464=CARTESIAN_POINT('Ctrl Pts',(89.0932918907188,3.67234351900059,-0.618085886174753));
#17465=CARTESIAN_POINT('Ctrl Pts',(89.084102188968,3.64162404748148,-0.775606014119531));
#17466=CARTESIAN_POINT('Ctrl Pts',(89.0804762276018,3.62770440805074,-0.83830305908965));
#17467=CARTESIAN_POINT('Ctrl Pts',(89.0752488758918,3.60483734450871,-0.930018155093909));
#17468=CARTESIAN_POINT('Ctrl Pts',(89.0735896779895,3.59714649009444,-0.95933482067506));
#17469=CARTESIAN_POINT('Ctrl Pts',(89.07058889883,3.58241797467355,-1.01280890788904));
#17470=CARTESIAN_POINT('Ctrl Pts',(89.0692418994431,3.57549244310308,-1.03699288710819));
#17471=CARTESIAN_POINT('Ctrl Pts',(89.0659934007909,3.55802841574153,-1.09572144579867));
#17472=CARTESIAN_POINT('Ctrl Pts',(89.0641057334838,3.54723158432662,-1.13018581169509));
#17473=CARTESIAN_POINT('Ctrl Pts',(89.0569367167298,3.50380542757732,-1.26204800350473));
#17474=CARTESIAN_POINT('Ctrl Pts',(89.0518189369649,3.46765012684196,-1.35824266117475));
#17475=CARTESIAN_POINT('Ctrl Pts',(89.0349855699098,3.33341721893172,-1.67493012477741));
#17476=CARTESIAN_POINT('Ctrl Pts',(89.023683582369,3.21790829069546,-1.88736171290549));
#17477=CARTESIAN_POINT('Ctrl Pts',(89.0075136338544,3.0321192529853,-2.16176904149654));
#17478=CARTESIAN_POINT('Ctrl Pts',(89.0030603253208,2.97889161431475,-2.23454605762287));
#17479=CARTESIAN_POINT('Ctrl Pts',(88.9948335641639,2.87772252040432,-2.36282562851171));
#17480=CARTESIAN_POINT('Ctrl Pts',(88.9910911700065,2.83068257878051,-2.41898059373968));
#17481=CARTESIAN_POINT('Ctrl Pts',(88.9848676364607,2.7511215014168,-2.50845771970211));
#17482=CARTESIAN_POINT('Ctrl Pts',(88.9824255227432,2.71957681224039,-2.5426229285879));
#17483=CARTESIAN_POINT('Ctrl Pts',(88.9775792497843,2.65641226263502,-2.60851429107209));
#17484=CARTESIAN_POINT('Ctrl Pts',(88.9751774219771,2.62484335254405,-2.64027840509861));
#17485=CARTESIAN_POINT('Ctrl Pts',(88.969171658286,2.54530597114271,-2.7174710352027));
#17486=CARTESIAN_POINT('Ctrl Pts',(88.9655397924824,2.49668797750549,-2.76220558799185));
#17487=CARTESIAN_POINT('Ctrl Pts',(88.9470850960456,2.24717863843847,-2.97981382718044));
#17488=CARTESIAN_POINT('Ctrl Pts',(88.9314822248832,2.02944322049996,-3.13216012224463));
#17489=CARTESIAN_POINT('Ctrl Pts',(88.906170933265,1.65405971034384,-3.33912468529458));
#17490=CARTESIAN_POINT('Ctrl Pts',(88.8965359133057,1.50563230882365,-3.40862806644198));
#17491=CARTESIAN_POINT('Ctrl Pts',(88.884642795626,1.30957450721378,-3.48512056870059));
#17492=CARTESIAN_POINT('Ctrl Pts',(88.8820350210653,1.26572753199235,-3.50128333212678));
#17493=CARTESIAN_POINT('Ctrl Pts',(88.8779885118063,1.19610701654822,-3.52546778220378));
#17494=CARTESIAN_POINT('Ctrl Pts',(88.8765217797147,1.17053179127583,-3.5340416653562));
#17495=CARTESIAN_POINT('Ctrl Pts',(88.8736418786013,1.11957848989705,-3.55050950673595));
#17496=CARTESIAN_POINT('Ctrl Pts',(88.872228406133,1.0942047082546,-3.55841114514145));
#17497=CARTESIAN_POINT('Ctrl Pts',(88.8684729008517,1.02589051638927,-3.57888501394662));
#17498=CARTESIAN_POINT('Ctrl Pts',(88.866156852475,0.982803286887197,-3.59095632487383));
#17499=CARTESIAN_POINT('Ctrl Pts',(88.8509584129739,0.694726520927777,-3.66609000663269));
#17500=CARTESIAN_POINT('Ctrl Pts',(88.8390667976081,0.44405234745131,-3.70482167298268));
#17501=CARTESIAN_POINT('Ctrl Pts',(88.8183654178315,0.0138108003517332,
-3.72696752168558));
#17502=CARTESIAN_POINT('Ctrl Pts',(88.809724245046,-0.164162344080656,-3.72337500708856));
#17503=CARTESIAN_POINT('Ctrl Pts',(88.7973539917731,-0.4074110144934,-3.70098724759685));
#17504=CARTESIAN_POINT('Ctrl Pts',(88.7939397649367,-0.473457085166123,
-3.69311901419517));
#17505=CARTESIAN_POINT('Ctrl Pts',(88.7881103829699,-0.584072730066627,
-3.67692511787763));
#17506=CARTESIAN_POINT('Ctrl Pts',(88.7857243619475,-0.628765992733442,
-3.66954661608876));
#17507=CARTESIAN_POINT('Ctrl Pts',(88.781130875323,-0.713628165726399,-3.6539407140514));
#17508=CARTESIAN_POINT('Ctrl Pts',(88.7789283040564,-0.753817710473505,
-3.64586156899731));
#17509=CARTESIAN_POINT('Ctrl Pts',(88.7730231059186,-0.860195246865727,
-3.62264282803465));
#17510=CARTESIAN_POINT('Ctrl Pts',(88.7692856344061,-0.926114235898302,
-3.60635391158795));
#17511=CARTESIAN_POINT('Ctrl Pts',(88.7558175497773,-1.15863765264743,-3.54210065517404));
#17512=CARTESIAN_POINT('Ctrl Pts',(88.7458003941647,-1.32228125109999,-3.48431911908711));
#17513=CARTESIAN_POINT('Ctrl Pts',(88.7207097738773,-1.71424589532725,-3.31431823997872));
#17514=CARTESIAN_POINT('Ctrl Pts',(88.7054904475159,-1.93625711959802,-3.18971159556248));
#17515=CARTESIAN_POINT('Ctrl Pts',(88.6886246738772,-2.18066475537463,-3.01754794215074));
#17516=CARTESIAN_POINT('Ctrl Pts',(88.6861158315554,-2.21699840101319,-2.9909551651464));
#17517=CARTESIAN_POINT('Ctrl Pts',(88.6821856526777,-2.27404496929703,-2.94759161994577));
#17518=CARTESIAN_POINT('Ctrl Pts',(88.6807388033406,-2.2950748920228,-2.93124687110775));
#17519=CARTESIAN_POINT('Ctrl Pts',(88.6778598228605,-2.3370243965377,-2.89791486339369));
#17520=CARTESIAN_POINT('Ctrl Pts',(88.6764280846079,-2.35793850266962,-2.88092340927177));
#17521=CARTESIAN_POINT('Ctrl Pts',(88.6725641530622,-2.41444352350375,-2.83398890250482));
#17522=CARTESIAN_POINT('Ctrl Pts',(88.6701605823034,-2.44966166347531,-2.80360281270346));
#17523=CARTESIAN_POINT('Ctrl Pts',(88.6588630634242,-2.61480297805074,-2.65563108924387));
#17524=CARTESIAN_POINT('Ctrl Pts',(88.6504219683624,-2.73689586753458,-2.52962092554381));
#17525=CARTESIAN_POINT('Ctrl Pts',(88.6307328282848,-3.00106509155236,-2.21536363321619));
#17526=CARTESIAN_POINT('Ctrl Pts',(88.6195323628153,-3.13503966291681,-2.02132292535156));
#17527=CARTESIAN_POINT('Ctrl Pts',(88.6039349864454,-3.28632488119421,-1.75058326728957));
#17528=CARTESIAN_POINT('Ctrl Pts',(88.6001134778783,-3.32086422689459,-1.68414157731951));
#17529=CARTESIAN_POINT('Ctrl Pts',(88.5937933316334,-3.3737057698613,-1.57453753931268));
#17530=CARTESIAN_POINT('Ctrl Pts',(88.5913362233642,-3.39323804458672,-1.53199033939784));
#17531=CARTESIAN_POINT('Ctrl Pts',(88.5864845423334,-3.42980995724489,-1.44819271146429));
#17532=CARTESIAN_POINT('Ctrl Pts',(88.5840928365297,-3.44692043440622,-1.40698179094277));
#17533=CARTESIAN_POINT('Ctrl Pts',(88.5781595289875,-3.48710994749023,-1.30504816430974));
#17534=CARTESIAN_POINT('Ctrl Pts',(88.5745915638923,-3.50934768756217,-1.24401149317139));
#17535=CARTESIAN_POINT('Ctrl Pts',(88.553966623892,-3.62699394460167,-0.892794377824449));
#17536=CARTESIAN_POINT('Ctrl Pts',(88.5358264700019,-3.68798470295983,-0.592353711252517));
#17537=CARTESIAN_POINT('Ctrl Pts',(88.5121769037604,-3.71907026873135,-0.191606689232467));
#17538=CARTESIAN_POINT('Ctrl Pts',(88.5065323665067,-3.72278981183138,-0.0950494822277428));
#17539=CARTESIAN_POINT('Ctrl Pts',(88.4973139553979,-3.72272295005873,0.0658804134627193));
#17540=CARTESIAN_POINT('Ctrl Pts',(88.4936798857592,-3.72102857088104,0.130206252110795));
#17541=CARTESIAN_POINT('Ctrl Pts',(88.4884465217943,-3.71608640439314,0.224690529694151));
#17542=CARTESIAN_POINT('Ctrl Pts',(88.4867888945916,-3.71413635131042,0.254902497261594));
#17543=CARTESIAN_POINT('Ctrl Pts',(88.4839293988324,-3.71008940424378,0.307593300712719));
#17544=CARTESIAN_POINT('Ctrl Pts',(88.4827193497549,-3.70815635433156,0.330081057069221));
#17545=CARTESIAN_POINT('Ctrl Pts',(88.4797113045783,-3.7027949605819,0.38643998925021));
#17546=CARTESIAN_POINT('Ctrl Pts',(88.4779268546235,-3.69910638263114,0.42028385159385));
#17547=CARTESIAN_POINT('Ctrl Pts',(88.4714594312061,-3.68388030997718,0.544183697253454));
#17548=CARTESIAN_POINT('Ctrl Pts',(88.4669047634828,-3.66951327957472,0.633864703046565));
#17549=CARTESIAN_POINT('Ctrl Pts',(88.4538739503025,-3.61813924745274,0.893378449656369));
#17550=CARTESIAN_POINT('Ctrl Pts',(88.44562527822,-3.57250571857085,1.06125601110274));
#17551=CARTESIAN_POINT('Ctrl Pts',(88.4284338128901,-3.45461863748153,1.39945659590232));
#17552=CARTESIAN_POINT('Ctrl Pts',(88.4194984320634,-3.38107645317056,1.56881596478263));
#17553=CARTESIAN_POINT('Ctrl Pts',(88.4067204799356,-3.26349299061986,1.79252714591052));
#17554=CARTESIAN_POINT('Ctrl Pts',(88.4032158750203,-3.23003119835978,1.85214410795675));
#17555=CARTESIAN_POINT('Ctrl Pts',(88.3972779647094,-3.17152755356454,1.94996478133264));
#17556=CARTESIAN_POINT('Ctrl Pts',(88.3948764007927,-3.14738933677125,1.98869047224285));
#17557=CARTESIAN_POINT('Ctrl Pts',(88.3899962656051,-3.09743808038409,2.06564067067064));
#17558=CARTESIAN_POINT('Ctrl Pts',(88.3875175776027,-3.07161437044837,2.10384860328771));
#17559=CARTESIAN_POINT('Ctrl Pts',(88.3811519324637,-3.00419673595804,2.1997096057063));
#17560=CARTESIAN_POINT('Ctrl Pts',(88.3772303670927,-2.96165025350118,2.25666728368062));
#17561=CARTESIAN_POINT('Ctrl Pts',(88.3684150657029,-2.86382866378502,2.38008812485602));
#17562=CARTESIAN_POINT('Ctrl Pts',(88.3634964901018,-2.8078174721378,2.44591366981495));
#17563=CARTESIAN_POINT('Ctrl Pts',(88.3549444113181,-2.70785514815031,2.55542887415017));
#17564=CARTESIAN_POINT('Ctrl Pts',(88.351345304935,-2.66502431353806,2.60006452616581));
#17565=CARTESIAN_POINT('Ctrl Pts',(88.3477258555205,-2.62111983094262,2.64359573201716));
#17566=CARTESIAN_POINT('',(88.2572559480606,-3.72274871244099,-0.00309621042271729));
#17567=CARTESIAN_POINT('Ctrl Pts',(88.1029424526342,-2.62112000712061,2.64359555733703));
#17568=CARTESIAN_POINT('Ctrl Pts',(88.1041532669587,-2.63620271695778,2.62864107899177));
#17569=CARTESIAN_POINT('Ctrl Pts',(88.105358311338,-2.65116024039027,2.6135547508114));
#17570=CARTESIAN_POINT('Ctrl Pts',(88.1090818796747,-2.69724005597925,2.56627515837679));
#17571=CARTESIAN_POINT('Ctrl Pts',(88.1115763284437,-2.72790974294777,2.53364971702599));
#17572=CARTESIAN_POINT('Ctrl Pts',(88.1154899655916,-2.77584500242704,2.48077793296012));
#17573=CARTESIAN_POINT('Ctrl Pts',(88.1169342969881,-2.79349439765197,2.46088678757825));
#17574=CARTESIAN_POINT('Ctrl Pts',(88.1198134978056,-2.82863138308299,2.42042165591336));
#17575=CARTESIAN_POINT('Ctrl Pts',(88.1212478706564,-2.84611124018731,2.3998432010622));
#17576=CARTESIAN_POINT('Ctrl Pts',(88.1251289890557,-2.89327084463644,2.34308367387563));
#17577=CARTESIAN_POINT('Ctrl Pts',(88.1275466613924,-2.92249551266324,2.30652934882947));
#17578=CARTESIAN_POINT('Ctrl Pts',(88.1382986841977,-3.05118439093271,2.13919056682107));
#17579=CARTESIAN_POINT('Ctrl Pts',(88.1462401225262,-3.14262052111368,2.00245028441192));
#17580=CARTESIAN_POINT('Ctrl Pts',(88.1668144288718,-3.35677608955448,1.63118478771012));
#17581=CARTESIAN_POINT('Ctrl Pts',(88.1793536890746,-3.46406346664572,1.38887158132868));
#17582=CARTESIAN_POINT('Ctrl Pts',(88.1960795984351,-3.56489226127524,1.07458863044898));
#17583=CARTESIAN_POINT('Ctrl Pts',(88.1994597821775,-3.58332838559592,1.01141217252422));
#17584=CARTESIAN_POINT('Ctrl Pts',(88.2052262966283,-3.61147194523394,0.904511005190628));
#17585=CARTESIAN_POINT('Ctrl Pts',(88.2075840319613,-3.62208249910761,0.861038856598137));
#17586=CARTESIAN_POINT('Ctrl Pts',(88.2124462260877,-3.6421329738008,0.771948335350112));
#17587=CARTESIAN_POINT('Ctrl Pts',(88.2149523062546,-3.65150536341464,0.726323033160018));
#17588=CARTESIAN_POINT('Ctrl Pts',(88.2200745264829,-3.66872512758083,0.633712597483294));
#17589=CARTESIAN_POINT('Ctrl Pts',(88.2226913962652,-3.67653162855893,0.586728746738759));
#17590=CARTESIAN_POINT('Ctrl Pts',(88.2354168265011,-3.70976514497697,0.359873053982928));
#17591=CARTESIAN_POINT('Ctrl Pts',(88.245881282912,-3.72290178407679,0.178473664449434));
#17592=CARTESIAN_POINT('Ctrl Pts',(88.2565361263338,-3.72274867707829,-0.00313844099074864));
#17593=CARTESIAN_POINT('Ctrl Pts',(88.2572559480606,-3.72274871244099,-0.00309621042271729));
#17594=CARTESIAN_POINT('Ctrl Pts',(88.2646021442827,-3.72263426646549,-0.140701072421199));
#17595=CARTESIAN_POINT('Ctrl Pts',(88.2719483405047,-3.71488660768827,-0.277983462742277));
#17596=CARTESIAN_POINT('Ctrl Pts',(88.2792945367267,-3.69963501555635,-0.414208056620568));
#17597=CARTESIAN_POINT('Ctrl Pts',(88.2867550257305,-3.68414613778178,-0.552552044987124));
#17598=CARTESIAN_POINT('Ctrl Pts',(88.2942155147343,-3.66091805396147,-0.689805171380509));
#17599=CARTESIAN_POINT('Ctrl Pts',(88.3016760037381,-3.63013505052346,-0.825219411708824));
#17600=CARTESIAN_POINT('Ctrl Pts',(88.3046127904125,-3.61801746490033,-0.878524595365555));
#17601=CARTESIAN_POINT('Ctrl Pts',(88.3075495770868,-3.60472971913711,-0.931545061605505));
#17602=CARTESIAN_POINT('Ctrl Pts',(88.3104863637612,-3.59028508188239,-0.98423604552605));
#17603=CARTESIAN_POINT('Ctrl Pts',(88.3164524120401,-3.56094096779148,-1.0912771720328));
#17604=CARTESIAN_POINT('Ctrl Pts',(88.3224184603191,-3.52675840703198,-1.19717735641402));
#17605=CARTESIAN_POINT('Ctrl Pts',(88.328384508598,-3.48784301668361,-1.30146788414905));
#17606=CARTESIAN_POINT('Ctrl Pts',(88.3343429893628,-3.44897698778097,-1.40562612665759));
#17607=CARTESIAN_POINT('Ctrl Pts',(88.3403014701276,-3.40539021220487,-1.50817838543764));
#17608=CARTESIAN_POINT('Ctrl Pts',(88.3462599508923,-3.3572386024678,-1.60866917935293));
#17609=CARTESIAN_POINT('Ctrl Pts',(88.3522124909595,-3.30913500063087,-1.70905978239142));
#17610=CARTESIAN_POINT('Ctrl Pts',(88.3581650310268,-3.25647579655805,-1.80739263475249));
#17611=CARTESIAN_POINT('Ctrl Pts',(88.364117571094,-3.19946543296315,-1.90323106998965));
#17612=CARTESIAN_POINT('Ctrl Pts',(88.3700659525545,-3.14249489836185,-1.99900254988424));
#17613=CARTESIAN_POINT('Ctrl Pts',(88.376014334015,-3.08117946358779,-2.09228272193326));
#17614=CARTESIAN_POINT('Ctrl Pts',(88.3819627154755,-3.01576972954598,-2.1826590436562));
#17615=CARTESIAN_POINT('Ctrl Pts',(88.3879088995304,-2.9503841586676,-2.27300197924993));
#17616=CARTESIAN_POINT('Ctrl Pts',(88.3938550835854,-2.88090753952243,-2.36044285979049));
#17617=CARTESIAN_POINT('Ctrl Pts',(88.3998012676404,-2.80763370279342,-2.44459823967836));
#17618=CARTESIAN_POINT('Ctrl Pts',(88.4057467165196,-2.73436892551189,-2.52874321474401));
#17619=CARTESIAN_POINT('Ctrl Pts',(88.4116921653989,-2.65730813807171,-2.60960318263874));
#17620=CARTESIAN_POINT('Ctrl Pts',(88.4176376142782,-2.57678485283428,-2.68682849930989));
#17621=CARTESIAN_POINT('Ctrl Pts',(88.423583789286,-2.49625173314121,-2.76406324764976));
#17622=CARTESIAN_POINT('Ctrl Pts',(88.4295299642938,-2.41225557608458,-2.83766217391017));
#17623=CARTESIAN_POINT('Ctrl Pts',(88.4354761393016,-2.32516550554824,-2.90731369726568));
#17624=CARTESIAN_POINT('Ctrl Pts',(88.441428237806,-2.23798867709732,-2.97703460649807));
#17625=CARTESIAN_POINT('Ctrl Pts',(88.4473803363105,-2.14771210457599,-3.04279999665133));
#17626=CARTESIAN_POINT('Ctrl Pts',(88.453332434815,-2.05473675010977,-3.10433961580371));
#17627=CARTESIAN_POINT('Ctrl Pts',(88.459287463955,-1.96171561735466,-3.16590953522739));
#17628=CARTESIAN_POINT('Ctrl Pts',(88.4652424930951,-1.86599341268227,-3.22324932332814));
#17629=CARTESIAN_POINT('Ctrl Pts',(88.4711975222352,-1.76799713788626,-3.27613395375189));
#17630=CARTESIAN_POINT('Ctrl Pts',(88.4771622299419,-1.66984159208639,-3.32910453630182));
#17631=CARTESIAN_POINT('Ctrl Pts',(88.4831269376485,-1.5694049662657,-3.37760530968939));
#17632=CARTESIAN_POINT('Ctrl Pts',(88.4890916453551,-1.46713619053383,-3.42145860137543));
#17633=CARTESIAN_POINT('Ctrl Pts',(88.4947508385346,-1.37010565918835,-3.46306571129821));
#17634=CARTESIAN_POINT('Ctrl Pts',(88.5004100317141,-1.27142630185272,-3.50048953684433));
#17635=CARTESIAN_POINT('Ctrl Pts',(88.5060692248936,-1.17149313307071,-3.5336201552612));
#17636=CARTESIAN_POINT('Ctrl Pts',(88.5120351479814,-1.06614355761611,-3.56854646278557));
#17637=CARTESIAN_POINT('Ctrl Pts',(88.5180010710692,-0.959060901017507,
-3.59881371921158));
#17638=CARTESIAN_POINT('Ctrl Pts',(88.523966994157,-0.850693777783829,-3.62424994432502));
#17639=CARTESIAN_POINT('Ctrl Pts',(88.5299253496939,-0.742464114205368,
-3.64965390453532));
#17640=CARTESIAN_POINT('Ctrl Pts',(88.5358837052307,-0.63295362662988,-3.67023892532855));
#17641=CARTESIAN_POINT('Ctrl Pts',(88.5418420607675,-0.522627803341301,
-3.68588222026622));
#17642=CARTESIAN_POINT('Ctrl Pts',(88.5477944757295,-0.412411976644462,
-3.70150991859128));
#17643=CARTESIAN_POINT('Ctrl Pts',(88.5537468906916,-0.301382841783696,
-3.71220563298313));
#17644=CARTESIAN_POINT('Ctrl Pts',(88.5596993056537,-0.190017136997689,
-3.71789739639856));
#17645=CARTESIAN_POINT('Ctrl Pts',(88.5656475627016,-0.0787292240061793,
-3.72358518397161));
#17646=CARTESIAN_POINT('Ctrl Pts',(88.5715958197495,0.0328943761053461,
-3.72427595236333));
#17647=CARTESIAN_POINT('Ctrl Pts',(88.5775440767974,0.144371408924188,-3.71994952368782));
#17648=CARTESIAN_POINT('Ctrl Pts',(88.5834901369028,0.255807268568044,-3.71562469294509));
#17649=CARTESIAN_POINT('Ctrl Pts',(88.5894361970082,0.367096252431375,-3.70628636522292));
#17650=CARTESIAN_POINT('Ctrl Pts',(88.5953822571136,0.477756352484418,-3.69196647197138));
#17651=CARTESIAN_POINT('Ctrl Pts',(88.6013275826489,0.588402781703338,-3.67764834778461));
#17652=CARTESIAN_POINT('Ctrl Pts',(88.6072729081842,0.69842006819559,-3.65834993549135));
#17653=CARTESIAN_POINT('Ctrl Pts',(88.6132182337196,0.807332333122118,-3.63415493153437));
#17654=CARTESIAN_POINT('Ctrl Pts',(88.6191642861319,0.916257913690046,-3.60995696949001));
#17655=CARTESIAN_POINT('Ctrl Pts',(88.6251103385442,1.02407779715116,-3.58086131636578));
#17656=CARTESIAN_POINT('Ctrl Pts',(88.6310563909565,1.1303280374453,-3.54700240911464));
#17657=CARTESIAN_POINT('Ctrl Pts',(88.6370083687989,1.23668415947741,-3.51310976038738));
#17658=CARTESIAN_POINT('Ctrl Pts',(88.6429603466413,1.34146711565789,-3.47444450230322));
#17659=CARTESIAN_POINT('Ctrl Pts',(88.6489123244836,1.44422970256022,-3.43119048272503));
#17660=CARTESIAN_POINT('Ctrl Pts',(88.6548672338371,1.54704290283419,-3.38791515936466));
#17661=CARTESIAN_POINT('Ctrl Pts',(88.6608221431906,1.64783337417348,-3.34004674994136));
#17662=CARTESIAN_POINT('Ctrl Pts',(88.666777052544,1.74617711412755,-3.28781584773192));
#17663=CARTESIAN_POINT('Ctrl Pts',(88.6727416432172,1.84468073849385,-3.23550003003012));
#17664=CARTESIAN_POINT('Ctrl Pts',(88.6787062338903,1.94072932268429,-3.17880775858277));
#17665=CARTESIAN_POINT('Ctrl Pts',(88.6846708245634,2.03392611576056,-3.11801413052077));
#17666=CARTESIAN_POINT('Ctrl Pts',(88.6903312450509,2.12237024643251,-3.0603207334965));
#17667=CARTESIAN_POINT('Ctrl Pts',(88.6959916655384,2.2082460307644,-2.9989341534039));
#17668=CARTESIAN_POINT('Ctrl Pts',(88.7016520860259,2.29124277537432,-2.93412237420238));
#17669=CARTESIAN_POINT('Ctrl Pts',(88.7076181048113,2.37872039979447,-2.8658114964006));
#17670=CARTESIAN_POINT('Ctrl Pts',(88.7135841235967,2.46328144756805,-2.79347504670955));
#17671=CARTESIAN_POINT('Ctrl Pts',(88.719550142382,2.54453405527325,-2.71739102891996));
#17672=CARTESIAN_POINT('Ctrl Pts',(88.725508592765,2.62568358713349,-2.64140353017932));
#17673=CARTESIAN_POINT('Ctrl Pts',(88.731467043148,2.70353272353865,-2.56167820019026));
#17674=CARTESIAN_POINT('Ctrl Pts',(88.737425493531,2.7777211860168,-2.47853436031326));
#17675=CARTESIAN_POINT('Ctrl Pts',(88.7433780023797,2.85183567065308,-2.39547342823124));
#17676=CARTESIAN_POINT('Ctrl Pts',(88.7493305112283,2.92229646595111,-2.30900107608306));
#17677=CARTESIAN_POINT('Ctrl Pts',(88.7552830200769,2.98877934918925,-2.2194741639316));
#17678=CARTESIAN_POINT('Ctrl Pts',(88.7612313691924,3.0552157728482,-2.13000981499135));
#17679=CARTESIAN_POINT('Ctrl Pts',(88.7671797183078,3.11767956629616,-2.03749548588472));
#17680=CARTESIAN_POINT('Ctrl Pts',(88.7731280674232,3.17588654864072,-1.94232134124684));
#17681=CARTESIAN_POINT('Ctrl Pts',(88.7790742184606,3.23407202190977,-1.84718236606427));
#17682=CARTESIAN_POINT('Ctrl Pts',(88.785020369498,3.28800359400462,-1.74938588457056));
#17683=CARTESIAN_POINT('Ctrl Pts',(88.7909665205354,3.33744058709227,-1.64935074806094));
#17684=CARTESIAN_POINT('Ctrl Pts',(88.796911935768,3.38687146261316,-1.54932799037107));
#17685=CARTESIAN_POINT('Ctrl Pts',(88.8028573510006,3.43180868055454,-1.44706750231301));
#17686=CARTESIAN_POINT('Ctrl Pts',(88.8088027662332,3.47205804118375,-1.34301173529917));
#17687=CARTESIAN_POINT('Ctrl Pts',(88.8147489070081,3.51231231360008,-1.23894326995253));
#17688=CARTESIAN_POINT('Ctrl Pts',(88.820695047783,3.54787744128388,-1.13307947907829));
#17689=CARTESIAN_POINT('Ctrl Pts',(88.8266411885579,3.57860806773621,-1.02588101650888));
#17690=CARTESIAN_POINT('Ctrl Pts',(88.8325932521278,3.60936930416032,-0.918575776359818));
#17691=CARTESIAN_POINT('Ctrl Pts',(88.8385453156978,3.63528630474838,-0.809933610416527));
#17692=CARTESIAN_POINT('Ctrl Pts',(88.8444973792677,3.65626411656129,-0.700428634798912));
#17693=CARTESIAN_POINT('Ctrl Pts',(88.8504523730391,3.67725225575308,-0.590869749870746));
#17694=CARTESIAN_POINT('Ctrl Pts',(88.8564073668105,3.69329630096893,-0.480447621677139));
#17695=CARTESIAN_POINT('Ctrl Pts',(88.862362360582,3.70435306530166,-0.369642976519477));
#17696=CARTESIAN_POINT('Ctrl Pts',(88.8683270325657,3.71542779937819,-0.258658248742223));
#17697=CARTESIAN_POINT('Ctrl Pts',(88.8742917045494,3.72149903216251,-0.147290178647985));
#17698=CARTESIAN_POINT('Ctrl Pts',(88.8802563765331,3.72257572318515,-0.0360214887612145));
#17699=CARTESIAN_POINT('Ctrl Pts',(88.8859159000748,3.72359733144901,0.0695547728663779));
#17700=CARTESIAN_POINT('Ctrl Pts',(88.8915754236166,3.72012280657342,0.175041267955078));
#17701=CARTESIAN_POINT('Ctrl Pts',(88.8972349471584,3.71220287368453,0.280031046686448));
#17702=CARTESIAN_POINT('Ctrl Pts',(88.9032012709903,3.70385360470569,0.390712275297176));
#17703=CARTESIAN_POINT('Ctrl Pts',(88.9091675948222,3.6905365666675,0.50119802511437));
#17704=CARTESIAN_POINT('Ctrl Pts',(88.9151339186541,3.67226589290483,0.611007998562921));
#17705=CARTESIAN_POINT('Ctrl Pts',(88.9210926761652,3.6540183894869,0.72067871415086));
#17706=CARTESIAN_POINT('Ctrl Pts',(88.9270514336763,3.63082981102373,0.829674949827213));
#17707=CARTESIAN_POINT('Ctrl Pts',(88.9330101911873,3.60276618805977,0.937519790016859));
#17708=CARTESIAN_POINT('Ctrl Pts',(88.9389630088252,3.57473053978036,1.04525712714507));
#17709=CARTESIAN_POINT('Ctrl Pts',(88.9449158264631,3.54182961757212,1.15184495044759));
#17710=CARTESIAN_POINT('Ctrl Pts',(88.950868644101,3.50418068271759,1.25681554150516));
#17711=CARTESIAN_POINT('Ctrl Pts',(88.9568173032376,3.46655804854129,1.36171280252696));
#17712=CARTESIAN_POINT('Ctrl Pts',(88.9627659623743,3.42419413993121,1.46499468741295));
#17713=CARTESIAN_POINT('Ctrl Pts',(88.9687146215109,3.37725613496972,1.56620833904989));
#17714=CARTESIAN_POINT('Ctrl Pts',(88.9746610832101,3.33033546892934,1.66738460231627));
#17715=CARTESIAN_POINT('Ctrl Pts',(88.9806075449093,3.27884424083381,1.76649377348942));
#17716=CARTESIAN_POINT('Ctrl Pts',(88.9865540066085,3.2229976213808,1.86310329694135));
#17717=CARTESIAN_POINT('Ctrl Pts',(88.9924997327737,3.16715790974735,1.95970087049975));
#17718=CARTESIAN_POINT('Ctrl Pts',(88.9984454589389,3.10696408677016,2.05379905038773));
#17719=CARTESIAN_POINT('Ctrl Pts',(89.0043911851041,3.04267673217578,2.14499087783052));
#17720=CARTESIAN_POINT('Ctrl Pts',(89.0103376367129,2.9783815338214,2.23619383167308));
#17721=CARTESIAN_POINT('Ctrl Pts',(89.0162840883218,2.90999205138104,2.32448938755635));
#17722=CARTESIAN_POINT('Ctrl Pts',(89.0222305399306,2.83781109306914,2.4095011439204));
#17723=CARTESIAN_POINT('Ctrl Pts',(89.0281829122409,2.7655582663663,2.49459754391186));
#17724=CARTESIAN_POINT('Ctrl Pts',(89.0341352845512,2.68950669308204,2.57640329466123));
#17725=CARTESIAN_POINT('Ctrl Pts',(89.0400876568615,2.60999833028177,2.6545764781649));
#17726=CARTESIAN_POINT('Ctrl Pts',(89.0460429586881,2.53045083668973,2.73278813533925));
#17727=CARTESIAN_POINT('Ctrl Pts',(89.0519982605147,2.44744347377688,2.80736338406813));
#17728=CARTESIAN_POINT('Ctrl Pts',(89.0579535623413,2.36135240111219,2.87799972207464));
#17729=CARTESIAN_POINT('Ctrl Pts',(89.0639185379399,2.27512148240209,2.94875080150818));
#17730=CARTESIAN_POINT('Ctrl Pts',(89.0698835135385,2.18579717817438,3.0155499338919));
#17731=CARTESIAN_POINT('Ctrl Pts',(89.0758484891371,2.09378622149929,3.07813690747499));
#17732=CARTESIAN_POINT('Ctrl Pts',(89.081504928855,2.00653449327098,3.13748659589294));
#17733=CARTESIAN_POINT('Ctrl Pts',(89.0871613685729,1.91686735019243,3.19304881204709));
#17734=CARTESIAN_POINT('Ctrl Pts',(89.0928178082907,1.82515095864938,3.24464043318227));
#17735=CARTESIAN_POINT('Ctrl Pts',(89.0987830432115,1.72842760457343,3.29904853357149));
#17736=CARTESIAN_POINT('Ctrl Pts',(89.1047482781323,1.62911316686676,3.34921567300339));
#17737=CARTESIAN_POINT('Ctrl Pts',(89.1107135130531,1.52761502358576,3.39488731804387));
#17738=CARTESIAN_POINT('Ctrl Pts',(89.1166711804925,1.4262456405835,3.44050102415506));
#17739=CARTESIAN_POINT('Ctrl Pts',(89.1226288479319,1.32269843816678,3.48163040728767));
#17740=CARTESIAN_POINT('Ctrl Pts',(89.1285865153713,1.21740676315428,3.51806599362863));
#17741=CARTESIAN_POINT('Ctrl Pts',(89.1345382431768,1.11222006110562,3.55446525467145));
#17742=CARTESIAN_POINT('Ctrl Pts',(89.1404899709822,1.00529273785723,3.58617989128365));
#17743=CARTESIAN_POINT('Ctrl Pts',(89.1464416987876,0.897078898501409,3.61304816081429));
#17744=CARTESIAN_POINT('Ctrl Pts',(89.1523892728783,0.788940581655154,3.63989767896197));
#17745=CARTESIAN_POINT('Ctrl Pts',(89.158336846969,0.679517938242419,3.66190745780231));
#17746=CARTESIAN_POINT('Ctrl Pts',(89.1642844210597,0.569280388242783,3.67896553423135));
#17747=CARTESIAN_POINT('Ctrl Pts',(89.1702298009894,0.459083506746855,3.6960173176464));
#17748=CARTESIAN_POINT('Ctrl Pts',(89.176175180919,0.348072727954916,3.70812096659158));
#17749=CARTESIAN_POINT('Ctrl Pts',(89.1821205608486,0.236727189724005,3.71521571381062));
#17750=CARTESIAN_POINT('Ctrl Pts',(89.1880652097681,0.125395341908594,3.72230958869981));
#17751=CARTESIAN_POINT('Ctrl Pts',(89.1940098586876,0.0137292326501387,
3.72439576015319));
#17752=CARTESIAN_POINT('Ctrl Pts',(89.199954507607,-0.0977881239321674,
3.72146544325187));
#17753=CARTESIAN_POINT('Ctrl Pts',(89.2058998877447,-0.209319197645145,
3.71853476590854));
#17754=CARTESIAN_POINT('Ctrl Pts',(89.2118452678825,-0.320701065401263,
3.71058638477275));
#17755=CARTESIAN_POINT('Ctrl Pts',(89.2177906480202,-0.431452730676845,
3.69766360066617));
#17756=CARTESIAN_POINT('Ctrl Pts',(89.2237419645574,-0.542314980325008,
3.68472791329562));
#17757=CARTESIAN_POINT('Ctrl Pts',(89.2296932810946,-0.652545355448581,
3.66680794954585));
#17758=CARTESIAN_POINT('Ctrl Pts',(89.2356445976319,-0.761669852515796,
3.64399870997076));
#17759=CARTESIAN_POINT('Ctrl Pts',(89.2415988506798,-0.87084819401371,3.62117821581441));
#17760=CARTESIAN_POINT('Ctrl Pts',(89.2475531037277,-0.9789191659806,3.59346374235548));
#17761=CARTESIAN_POINT('Ctrl Pts',(89.2535073567756,-1.08542260946939,3.56100060676106));
#17762=CARTESIAN_POINT('Ctrl Pts',(89.2594713065714,-1.19209949823035,3.52848460360477));
#17763=CARTESIAN_POINT('Ctrl Pts',(89.2654352563672,-1.29720336343462,3.49120462383835));
#17764=CARTESIAN_POINT('Ctrl Pts',(89.271399206163,-1.40029229414812,3.44935487496567));
#17765=CARTESIAN_POINT('Ctrl Pts',(89.277066360583,-1.49825101435125,3.40958777473466));
#17766=CARTESIAN_POINT('Ctrl Pts',(89.2827335150031,-1.59439024991325,3.36569493467304));
#17767=CARTESIAN_POINT('Ctrl Pts',(89.2884006694231,-1.68835254050114,3.31788083895178));
#17768=CARTESIAN_POINT('Ctrl Pts',(89.2943662008,-1.78726196685464,3.26754932032008));
#17769=CARTESIAN_POINT('Ctrl Pts',(89.3003317321768,-1.8840781706993,3.2127099734771));
#17770=CARTESIAN_POINT('Ctrl Pts',(89.3062972635537,-1.97836354151181,3.15356072719662));
#17771=CARTESIAN_POINT('Ctrl Pts',(89.3122561474734,-2.07254384909974,3.09447739157113));
#17772=CARTESIAN_POINT('Ctrl Pts',(89.3182150313931,-2.16419857771386,3.03109391957071));
#17773=CARTESIAN_POINT('Ctrl Pts',(89.3241739153128,-2.25291301874604,2.96365492128631));
#17774=CARTESIAN_POINT('Ctrl Pts',(89.3301264569248,-2.34153303701452,2.89628770135644));
#17775=CARTESIAN_POINT('Ctrl Pts',(89.3360789985367,-2.42721866449201,2.82487379474726));
#17776=CARTESIAN_POINT('Ctrl Pts',(89.3420315401486,-2.50958348575806,2.74970149116416));
#17777=CARTESIAN_POINT('Ctrl Pts',(89.344770091734,-2.54747659538451,2.71511740178278));
#17778=CARTESIAN_POINT('Ctrl Pts',(89.3475086433194,-2.58466723458277,2.67973841252858));
#17779=CARTESIAN_POINT('Ctrl Pts',(89.3502471949048,-2.62112000711957,2.64359555733806));
#17780=CARTESIAN_POINT('Origin',(81.4430005297901,0.,0.));
#17781=CARTESIAN_POINT('',(82.8471929193648,-4.43299894467431,0.00305884233546028));
#17782=CARTESIAN_POINT('',(82.4431778927679,1.9715882987731,3.9704317876197));
#17783=CARTESIAN_POINT('Ctrl Pts',(82.8471929193386,-4.43299894467391,0.00305884291686582));
#17784=CARTESIAN_POINT('Ctrl Pts',(82.838350910046,-4.43286333405117,0.199591245476362));
#17785=CARTESIAN_POINT('Ctrl Pts',(82.8295089007534,-4.41965490319418,0.395644430212545));
#17786=CARTESIAN_POINT('Ctrl Pts',(82.8206668914608,-4.39358256713249,0.589848476974774));
#17787=CARTESIAN_POINT('Ctrl Pts',(82.8188675761831,-4.38827694585923,0.629368262214482));
#17788=CARTESIAN_POINT('Ctrl Pts',(82.8170682609054,-4.3824387600355,0.668811577215154));
#17789=CARTESIAN_POINT('Ctrl Pts',(82.8152689456277,-4.37606998213278,0.708167008181277));
#17790=CARTESIAN_POINT('Ctrl Pts',(82.8095434643006,-4.35580431807122,0.833397304344789));
#17791=CARTESIAN_POINT('Ctrl Pts',(82.8038179829734,-4.33012882713862,0.957942294294973));
#17792=CARTESIAN_POINT('Ctrl Pts',(82.7980925016463,-4.29910184415742,1.08130122239931));
#17793=CARTESIAN_POINT('Ctrl Pts',(82.792373877528,-4.26811202110914,1.20451240782769));
#17794=CARTESIAN_POINT('Ctrl Pts',(82.7866552534097,-4.23178355475547,1.32653997614935));
#17795=CARTESIAN_POINT('Ctrl Pts',(82.7809366292914,-4.19022620725604,1.44689091918662));
#17796=CARTESIAN_POINT('Ctrl Pts',(82.7752234540714,-4.14870845700185,1.56712718777775));
#17797=CARTESIAN_POINT('Ctrl Pts',(82.7695102788515,-4.10197186958025,1.68568963731331));
#17798=CARTESIAN_POINT('Ctrl Pts',(82.7637971036315,-4.05017655073995,1.80209847340156));
#17799=CARTESIAN_POINT('Ctrl Pts',(82.7577924778341,-3.99573895768253,1.92444576248378));
#17800=CARTESIAN_POINT('Ctrl Pts',(82.7517878520368,-3.9357130141655,2.04441348614045));
#17801=CARTESIAN_POINT('Ctrl Pts',(82.7457832262395,-3.87034305857968,2.16146561594306));
#17802=CARTESIAN_POINT('Ctrl Pts',(82.7400762563077,-3.80821356316094,2.27271534369876));
#17803=CARTESIAN_POINT('Ctrl Pts',(82.734369286376,-3.74125734116528,2.38133119183427));
#17804=CARTESIAN_POINT('Ctrl Pts',(82.7286623164443,-3.66973201008125,2.48687675090364));
#17805=CARTESIAN_POINT('Ctrl Pts',(82.7229561860919,-3.5982172014279,2.59240678266523));
#17806=CARTESIAN_POINT('Ctrl Pts',(82.7172500557396,-3.52213484344504,2.69486709560078));
#17807=CARTESIAN_POINT('Ctrl Pts',(82.7115439253873,-3.44178611010701,2.79384991942561));
#17808=CARTESIAN_POINT('Ctrl Pts',(82.705837369286,-3.36143138174511,2.89284012861131));
#17809=CARTESIAN_POINT('Ctrl Pts',(82.7001308131848,-3.27680989489711,2.98835202452487));
#17810=CARTESIAN_POINT('Ctrl Pts',(82.6944242570835,-3.18826305183751,3.08001099223489));
#17811=CARTESIAN_POINT('Ctrl Pts',(82.6887160099204,-3.0996899691001,3.17169712185942));
#17812=CARTESIAN_POINT('Ctrl Pts',(82.6830077627572,-3.00718949135207,3.259527766406));
#17813=CARTESIAN_POINT('Ctrl Pts',(82.677299515594,-2.91113944295518,3.34316558723474));
#17814=CARTESIAN_POINT('Ctrl Pts',(82.6715852762598,-2.8149885670524,3.42689120596689));
#17815=CARTESIAN_POINT('Ctrl Pts',(82.6658710369255,-2.71528098050195,3.50641495259866));
#17816=CARTESIAN_POINT('Ctrl Pts',(82.6601567975912,-2.61242735439016,3.58143997828165));
#17817=CARTESIAN_POINT('Ctrl Pts',(82.6544390802149,-2.50951112515441,3.65651066886883));
#17818=CARTESIAN_POINT('Ctrl Pts',(82.6487213628387,-2.40344537098648,3.72707696357266));
#17819=CARTESIAN_POINT('Ctrl Pts',(82.6430036454624,-2.29466821463525,3.79288633954969));
#17820=CARTESIAN_POINT('Ctrl Pts',(82.6372780135051,-2.18574048672624,3.8587868102068));
#17821=CARTESIAN_POINT('Ctrl Pts',(82.6315523815478,-2.07409420998285,3.91991702478709));
#17822=CARTESIAN_POINT('Ctrl Pts',(82.6258267495906,-1.96019076016078,3.9760710737838));
#17823=CARTESIAN_POINT('Ctrl Pts',(82.6237798612255,-1.91947077537578,3.99614590052816));
#17824=CARTESIAN_POINT('Ctrl Pts',(82.6217329728604,-1.87846248902875,4.0155852111556));
#17825=CARTESIAN_POINT('Ctrl Pts',(82.6196860844953,-1.83718750489339,4.03438112625265));
#17826=CARTESIAN_POINT('Ctrl Pts',(82.6140967735162,-1.72448046823902,4.08570596467894));
#17827=CARTESIAN_POINT('Ctrl Pts',(82.608507462537,-1.60940687031023,4.13240137103484));
#17828=CARTESIAN_POINT('Ctrl Pts',(82.6029181515579,-1.49239253067008,4.17423688048488));
#17829=CARTESIAN_POINT('Ctrl Pts',(82.5973357789645,-1.37552344875908,4.21602045671786));
#17830=CARTESIAN_POINT('Ctrl Pts',(82.591753406371,-1.25671880267868,4.25295598841567));
#17831=CARTESIAN_POINT('Ctrl Pts',(82.5861710337776,-1.13642768496985,4.28485952124852));
#17832=CARTESIAN_POINT('Ctrl Pts',(82.5805940635969,-1.0162529805341,4.31673217902799));
#17833=CARTESIAN_POINT('Ctrl Pts',(82.5750170934162,-0.894595065335974,
4.34358241337939));
#17834=CARTESIAN_POINT('Ctrl Pts',(82.5694401232355,-0.771920950848933,
4.36527513974096));
#17835=CARTESIAN_POINT('Ctrl Pts',(82.5638668802236,-0.649328821226295,
4.3869533685434));
#17836=CARTESIAN_POINT('Ctrl Pts',(82.5582936372118,-0.525722252229353,
4.40348087016432));
#17837=CARTESIAN_POINT('Ctrl Pts',(82.5527203942,-0.401580620582193,4.41477315444099));
#17838=CARTESIAN_POINT('Ctrl Pts',(82.5471490536151,-0.277481364689749,
4.42606158409562));
#17839=CARTESIAN_POINT('Ctrl Pts',(82.5415777130302,-0.152847824230017,
4.43211830966476));
#17840=CARTESIAN_POINT('Ctrl Pts',(82.5360063724452,-0.0281660667782649,
4.43291051936335));
#17841=CARTESIAN_POINT('Ctrl Pts',(82.5304355573441,0.09650393080331,4.43370265434144));
#17842=CARTESIAN_POINT('Ctrl Pts',(82.524864742243,0.2212217189773,4.42923125828579));
#17843=CARTESIAN_POINT('Ctrl Pts',(82.5192939271418,0.345500417941909,4.41951563649253));
#17844=CARTESIAN_POINT('Ctrl Pts',(82.513722261215,0.469798097883816,4.40979853084083));
#17845=CARTESIAN_POINT('Ctrl Pts',(82.5081505952881,0.593656139356998,4.39483564139945));
#17846=CARTESIAN_POINT('Ctrl Pts',(82.5025789293612,0.716592740410878,4.37469814323119));
#17847=CARTESIAN_POINT('Ctrl Pts',(82.4970019744931,0.839646039857502,4.35454152940779));
#17848=CARTESIAN_POINT('Ctrl Pts',(82.491425019625,0.961775740501727,4.32920056909857));
#17849=CARTESIAN_POINT('Ctrl Pts',(82.4858480647569,1.08251016603548,4.29879759240068));
#17850=CARTESIAN_POINT('Ctrl Pts',(82.4802681803071,1.20330801352119,4.26837864497927));
#17851=CARTESIAN_POINT('Ctrl Pts',(82.4746882958573,1.32270872795416,4.23289250833582));
#17852=CARTESIAN_POINT('Ctrl Pts',(82.4691084114075,1.44025740494804,4.19251089533376));
#17853=CARTESIAN_POINT('Ctrl Pts',(82.4635205574568,1.55797397149176,4.15207160706898));
#17854=CARTESIAN_POINT('Ctrl Pts',(82.457932703506,1.67383283321428,4.10672303810115));
#17855=CARTESIAN_POINT('Ctrl Pts',(82.4523448495553,1.78740045057869,4.05668443797039));
#17856=CARTESIAN_POINT('Ctrl Pts',(82.4492891972928,1.84950356744689,4.02932141756052));
#17857=CARTESIAN_POINT('Ctrl Pts',(82.4462335450304,1.91092196963203,4.00055672895153));
#17858=CARTESIAN_POINT('Ctrl Pts',(82.4431778927679,1.9715882987731,3.9704317876197));
#17859=CARTESIAN_POINT('',(82.4430005297901,-1.97158113240048,3.97043534620102));
#17860=CARTESIAN_POINT('Origin',(82.4430005297901,0.,0.));
#17861=CARTESIAN_POINT('',(82.6638081402658,-4.43299984791433,0.00116120262292478));
#17862=CARTESIAN_POINT('Ctrl Pts',(82.4430005297901,-1.97158113240048,3.97043534620102));
#17863=CARTESIAN_POINT('Ctrl Pts',(82.4494638984827,-2.10057436133302,3.90638176159495));
#17864=CARTESIAN_POINT('Ctrl Pts',(82.4559272671753,-2.22637526730531,3.83607233314734));
#17865=CARTESIAN_POINT('Ctrl Pts',(82.4623906358678,-2.34842827658618,3.75983691531035));
#17866=CARTESIAN_POINT('Ctrl Pts',(82.4689240795752,-2.47180456894732,3.68277496284602));
#17867=CARTESIAN_POINT('Ctrl Pts',(82.4754575232826,-2.59135104040891,3.59965787543973));
#17868=CARTESIAN_POINT('Ctrl Pts',(82.4819909669899,-2.7065244273022,3.51087090682875));
#17869=CARTESIAN_POINT('Ctrl Pts',(82.4884591884542,-2.82054805811389,3.42297028323097));
#17870=CARTESIAN_POINT('Ctrl Pts',(82.4949274099185,-2.93028537609616,3.32951260882839));
#17871=CARTESIAN_POINT('Ctrl Pts',(82.5013956313828,-3.03524125502932,3.23091310990687));
#17872=CARTESIAN_POINT('Ctrl Pts',(82.5079616862117,-3.14178461621387,3.1308222704704));
#17873=CARTESIAN_POINT('Ctrl Pts',(82.5145277410406,-3.24340054762542,3.02543291106605));
#17874=CARTESIAN_POINT('Ctrl Pts',(82.5210937958695,-3.33960719737278,2.9152208779535));
#17875=CARTESIAN_POINT('Ctrl Pts',(82.5276598506984,-3.43581384712013,2.80500884484095));
#17876=CARTESIAN_POINT('Ctrl Pts',(82.5342259055274,-3.52661104005606,2.68997426850115));
#17877=CARTESIAN_POINT('Ctrl Pts',(82.5407919603563,-3.61155585484342,2.57063286125153));
#17878=CARTESIAN_POINT('Ctrl Pts',(82.5465587614237,-3.68616075251107,2.46581830020199));
#17879=CARTESIAN_POINT('Ctrl Pts',(82.5523255624912,-3.7562202228349,2.35772393653131));
#17880=CARTESIAN_POINT('Ctrl Pts',(82.5580923635586,-3.82144896825721,2.24677920210373));
#17881=CARTESIAN_POINT('Ctrl Pts',(82.5638586415672,-3.88667179731824,2.13584453055759));
#17882=CARTESIAN_POINT('Ctrl Pts',(82.5696249195757,-3.94706457906038,2.02206033693403));
#17883=CARTESIAN_POINT('Ctrl Pts',(82.5753911975842,-4.0023868138301,1.90588268067027));
#17884=CARTESIAN_POINT('Ctrl Pts',(82.5811602666648,-4.05773582641746,1.78964879052325));
#17885=CARTESIAN_POINT('Ctrl Pts',(82.5869293357453,-4.10800922004284,1.67101947165996));
#17886=CARTESIAN_POINT('Ctrl Pts',(82.5926984048258,-4.15301362796875,1.55047309099703));
#17887=CARTESIAN_POINT('Ctrl Pts',(82.5984688920149,-4.19802909853494,1.42989707854227));
#17888=CARTESIAN_POINT('Ctrl Pts',(82.604239379204,-4.23777287589598,1.307403430887));
#17889=CARTESIAN_POINT('Ctrl Pts',(82.6100098663931,-4.27210103753376,1.18348710390227));
#17890=CARTESIAN_POINT('Ctrl Pts',(82.6157858342638,-4.30646180330307,1.05945308392053));
#17891=CARTESIAN_POINT('Ctrl Pts',(82.6215618021345,-4.33539658350209,0.933994060690117));
#17892=CARTESIAN_POINT('Ctrl Pts',(82.6273377700051,-4.35881219075801,0.807617041486446));
#17893=CARTESIAN_POINT('Ctrl Pts',(82.6310863103109,-4.37400866510629,0.725599730999895));
#17894=CARTESIAN_POINT('Ctrl Pts',(82.6348348506167,-4.3868815826507,0.643195975333012));
#17895=CARTESIAN_POINT('Ctrl Pts',(82.6385833909225,-4.39741715450987,0.560545599592328));
#17896=CARTESIAN_POINT('Ctrl Pts',(82.6469916406956,-4.42104921191562,0.375154768395029));
#17897=CARTESIAN_POINT('Ctrl Pts',(82.6553998904686,-4.43295082854589,0.188297149485439));
#17898=CARTESIAN_POINT('Ctrl Pts',(82.6638081402417,-4.43299984791419,0.00116120315987237));
#17899=CARTESIAN_POINT('',(83.91380814028,-4.43299997457298,-0.000474800938941028));
#17900=CARTESIAN_POINT('Ctrl Pts',(82.6638081402658,-4.43299984791433,0.00116120262292773));
#17901=CARTESIAN_POINT('Ctrl Pts',(82.66952634519,-4.43303318453861,-0.126104485083569));
#17902=CARTESIAN_POINT('Ctrl Pts',(82.6752445501142,-4.42758176932235,-0.253494044019376));
#17903=CARTESIAN_POINT('Ctrl Pts',(82.6809627550384,-4.41663987684345,-0.380501246090336));
#17904=CARTESIAN_POINT('Ctrl Pts',(82.6866768648111,-4.40570582051381,-0.507417490642293));
#17905=CARTESIAN_POINT('Ctrl Pts',(82.6923909745838,-4.38928914747985,-0.633951529973464));
#17906=CARTESIAN_POINT('Ctrl Pts',(82.6981050843566,-4.36743618383699,-0.759598696754644));
#17907=CARTESIAN_POINT('Ctrl Pts',(82.7038171800945,-4.34559092264133,-0.885201577063616));
#17908=CARTESIAN_POINT('Ctrl Pts',(82.7095292758324,-4.31831324733326,-1.00991781644859));
#17909=CARTESIAN_POINT('Ctrl Pts',(82.7152413715703,-4.28570112928413,-1.13324967701418));
#17910=CARTESIAN_POINT('Ctrl Pts',(82.7209525265382,-4.25309438238174,-1.25656122508364));
#17911=CARTESIAN_POINT('Ctrl Pts',(82.7266636815061,-4.21515504130049,-1.37848846485092));
#17912=CARTESIAN_POINT('Ctrl Pts',(82.732374836474,-4.17203169315451,-1.49854614587417));
#17913=CARTESIAN_POINT('Ctrl Pts',(82.7380863123118,-4.12890592220823,-1.61861057210152));
#17914=CARTESIAN_POINT('Ctrl Pts',(82.7437977881496,-4.08059569829891,-1.73680485750822));
#17915=CARTESIAN_POINT('Ctrl Pts',(82.7495092639875,-4.02729859725175,-1.85266160120355));
#17916=CARTESIAN_POINT('Ctrl Pts',(82.755222322258,-3.97398672960537,-1.96855044439523));
#17917=CARTESIAN_POINT('Ctrl Pts',(82.7609353805286,-3.91568540085796,-2.08210009715756));
#17918=CARTESIAN_POINT('Ctrl Pts',(82.7666484387991,-3.85263896726242,-2.19286615823473));
#17919=CARTESIAN_POINT('Ctrl Pts',(82.7723680894829,-3.78951978311419,-2.30376003450624));
#17920=CARTESIAN_POINT('Ctrl Pts',(82.7780877401667,-3.72164475296699,-2.41186355794363));
#17921=CARTESIAN_POINT('Ctrl Pts',(82.7838073908506,-3.64930283253258,-2.5167593918509));
#17922=CARTESIAN_POINT('Ctrl Pts',(82.7895303907495,-3.57691855135525,-2.62171664886426));
#17923=CARTESIAN_POINT('Ctrl Pts',(82.7952533906484,-3.50006240656649,-2.72346215752109));
#17924=CARTESIAN_POINT('Ctrl Pts',(82.8009763905473,-3.41906405993374,-2.82161123368713));
#17925=CARTESIAN_POINT('Ctrl Pts',(82.8067090419939,-3.33792911371723,-2.91992583326824));
#17926=CARTESIAN_POINT('Ctrl Pts',(82.8124416934405,-3.2526382714049,-3.01463158537872));
#17927=CARTESIAN_POINT('Ctrl Pts',(82.8181743448871,-3.16355907605327,-3.10537968247378));
#17928=CARTESIAN_POINT('Ctrl Pts',(82.8235049806097,-3.08072676969314,-3.18976385490041));
#17929=CARTESIAN_POINT('Ctrl Pts',(82.8288356163323,-2.99461937718249,-3.27072621832306));
#17930=CARTESIAN_POINT('Ctrl Pts',(82.8341662520549,-2.90555695574893,-3.34801848514894));
#17931=CARTESIAN_POINT('Ctrl Pts',(82.839824058202,-2.8110282838068,-3.43005460337752));
#17932=CARTESIAN_POINT('Ctrl Pts',(82.8454818643491,-2.71284674301988,-3.50823656309188));
#17933=CARTESIAN_POINT('Ctrl Pts',(82.8511396704962,-2.61136200335535,-3.5822168398119));
#17934=CARTESIAN_POINT('Ctrl Pts',(82.8567897948495,-2.51001505293713,-3.65609667102054));
#17935=CARTESIAN_POINT('Ctrl Pts',(82.8624399192028,-2.40537414749344,-3.72578592549306));
#17936=CARTESIAN_POINT('Ctrl Pts',(82.8680900435561,-2.29782447308528,-3.79097503168912));
#17937=CARTESIAN_POINT('Ctrl Pts',(82.8737339750989,-2.19039267834028,-3.85609268746079));
#17938=CARTESIAN_POINT('Ctrl Pts',(82.8793779066417,-2.08005880157589,-3.91671979497149));
#17939=CARTESIAN_POINT('Ctrl Pts',(82.8850218381844,-1.9672391924985,-3.97258844577409));
#17940=CARTESIAN_POINT('Ctrl Pts',(82.8906610595198,-1.85451373831238,-4.02841047075708));
#17941=CARTESIAN_POINT('Ctrl Pts',(82.8963002808551,-1.73930704246086,-4.07948175888407));
#17942=CARTESIAN_POINT('Ctrl Pts',(82.9019395021905,-1.62206187633748,-4.1255792647012));
#17943=CARTESIAN_POINT('Ctrl Pts',(82.9075758918359,-1.5048755839357,-4.17165362302481));
#17944=CARTESIAN_POINT('Ctrl Pts',(82.9132122814814,-1.38565323531322,-4.2127590163154));
#17945=CARTESIAN_POINT('Ctrl Pts',(82.9188486711269,-1.26485905207188,-4.24871987525558));
#17946=CARTESIAN_POINT('Ctrl Pts',(82.9244837033836,-1.14409395920267,-4.28467207388829));
#17947=CARTESIAN_POINT('Ctrl Pts',(82.9301187356403,-1.02175817495687,-4.31548208507233));
#17948=CARTESIAN_POINT('Ctrl Pts',(82.935753767897,-0.898332042706435,-4.34102390468503));
#17949=CARTESIAN_POINT('Ctrl Pts',(82.9413887767732,-0.774906422566319,
-4.36656561832156));
#17950=CARTESIAN_POINT('Ctrl Pts',(82.9470237856495,-0.650390862901795,
-4.38683910150858));
#17951=CARTESIAN_POINT('Ctrl Pts',(82.9526587945257,-0.525276262369073,
-4.40176939970639));
#17952=CARTESIAN_POINT('Ctrl Pts',(82.9582951137571,-0.400132567904806,
-4.41670316976977));
#17953=CARTESIAN_POINT('Ctrl Pts',(82.9639314329885,-0.274389960519799,
-4.42629123631845));
#17954=CARTESIAN_POINT('Ctrl Pts',(82.9695677522199,-0.1485441952278,-4.43051053740583));
#17955=CARTESIAN_POINT('Ctrl Pts',(82.9752099321354,-0.0225675746294041,
-4.43473422575198));
#17956=CARTESIAN_POINT('Ctrl Pts',(82.980852112051,0.103512009964471,-4.43357798956721));
#17957=CARTESIAN_POINT('Ctrl Pts',(82.9864942919665,0.22919885795583,-4.4270709146694));
#17958=CARTESIAN_POINT('Ctrl Pts',(82.9921397286903,0.35495825556051,-4.42056008372411));
#17959=CARTESIAN_POINT('Ctrl Pts',(82.9977851654142,0.480324059807185,-4.40869230250852));
#17960=CARTESIAN_POINT('Ctrl Pts',(83.003430602138,0.604807415447957,-4.39154835908921));
#17961=CARTESIAN_POINT('Ctrl Pts',(83.0090844057058,0.729475262183915,-4.37437900741447));
#17962=CARTESIAN_POINT('Ctrl Pts',(83.0147382092735,0.853257648687448,-4.35191795361543));
#17963=CARTESIAN_POINT('Ctrl Pts',(83.0203920128412,0.975677264387951,-4.32429680708395));
#17964=CARTESIAN_POINT('Ctrl Pts',(83.0235110462899,1.0432124858663,-4.3090590509628));
#17965=CARTESIAN_POINT('Ctrl Pts',(83.0266300797386,1.11033323896754,-4.29225175525319));
#17966=CARTESIAN_POINT('Ctrl Pts',(83.0297491131872,1.1769618225775,-4.27390335269705));
#17967=CARTESIAN_POINT('Ctrl Pts',(83.0354745794598,1.29926884958629,-4.24022203387839));
#17968=CARTESIAN_POINT('Ctrl Pts',(83.0412000457323,1.42030983933144,-4.20123662023261));
#17969=CARTESIAN_POINT('Ctrl Pts',(83.0469255120049,1.53959327565377,-4.15705924248882));
#17970=CARTESIAN_POINT('Ctrl Pts',(83.0526441242172,1.65873391559655,-4.11293475029054));
#17971=CARTESIAN_POINT('Ctrl Pts',(83.0583627364296,1.77612081943256,-4.06363079762116));
#17972=CARTESIAN_POINT('Ctrl Pts',(83.0640813486419,1.89127573333345,-4.00930980350783));
#17973=CARTESIAN_POINT('Ctrl Pts',(83.0697945150905,2.00632098663147,-3.95504053860658));
#17974=CARTESIAN_POINT('Ctrl Pts',(83.075507681539,2.11913812300309,-3.89576390865514));
#17975=CARTESIAN_POINT('Ctrl Pts',(83.0812208479875,2.22926746805393,-3.83169095255299));
#17976=CARTESIAN_POINT('Ctrl Pts',(83.0872254782513,2.34501518942459,-3.76434924025204));
#17977=CARTESIAN_POINT('Ctrl Pts',(83.0932301085152,2.45779323152163,-3.69170908293691));
#17978=CARTESIAN_POINT('Ctrl Pts',(83.099234738779,2.56709511962265,-3.6140713394743));
#17979=CARTESIAN_POINT('Ctrl Pts',(83.1049417078618,2.67097870090478,-3.54028224970026));
#17980=CARTESIAN_POINT('Ctrl Pts',(83.1106486769446,2.77172211169826,-3.4619793890988));
#17981=CARTESIAN_POINT('Ctrl Pts',(83.1163556460274,2.86891935081674,-3.37946604636136));
#17982=CARTESIAN_POINT('Ctrl Pts',(83.1220617784329,2.96610234021447,-3.29696480059398));
#17983=CARTESIAN_POINT('Ctrl Pts',(83.1277679108385,3.05973988983671,-3.21025455741205));
#17984=CARTESIAN_POINT('Ctrl Pts',(83.1334740432441,3.14945917911302,-3.11967881024646));
#17985=CARTESIAN_POINT('Ctrl Pts',(83.1391806042983,3.23918520816516,-3.02909625896731));
#17986=CARTESIAN_POINT('Ctrl Pts',(83.1448871653525,3.32499211215973,-2.93464790798709));
#17987=CARTESIAN_POINT('Ctrl Pts',(83.1505937264068,3.40654438100098,-2.83671365849122));
#17988=CARTESIAN_POINT('Ctrl Pts',(83.1563019814222,3.48812085818393,-2.73875033775294));
#17989=CARTESIAN_POINT('Ctrl Pts',(83.1620102364376,3.56543993364672,-2.63729936448726));
#17990=CARTESIAN_POINT('Ctrl Pts',(83.1677184914531,3.63820709300359,-2.53277281816162));
#17991=CARTESIAN_POINT('Ctrl Pts',(83.173432742932,3.71105069351727,-2.42813646776792));
#17992=CARTESIAN_POINT('Ctrl Pts',(83.179146994411,3.77933260400223,-2.32041841957391));
#17993=CARTESIAN_POINT('Ctrl Pts',(83.1848612458899,3.84280211367408,-2.21005902978677));
#17994=CARTESIAN_POINT('Ctrl Pts',(83.1905789779027,3.90631028243734,-2.09963242042033));
#17995=CARTESIAN_POINT('Ctrl Pts',(83.1962967099154,3.96500002782284,-1.98656161562392));
#17996=CARTESIAN_POINT('Ctrl Pts',(83.2020144419281,4.01866767330937,-1.87130946972921));
#17997=CARTESIAN_POINT('Ctrl Pts',(83.2077400921353,4.07240964037243,-1.75589771703413));
#17998=CARTESIAN_POINT('Ctrl Pts',(83.2134657423425,4.12111546961183,-1.63829895735629));
#17999=CARTESIAN_POINT('Ctrl Pts',(83.2191913925498,4.16463033859644,-1.51899412205647));
#18000=CARTESIAN_POINT('Ctrl Pts',(83.2212382531397,4.18018645312964,-1.47634388029783));
#18001=CARTESIAN_POINT('Ctrl Pts',(83.2232851137297,4.1950796382993,-1.4334757262206));
#18002=CARTESIAN_POINT('Ctrl Pts',(83.2253319743196,4.20930439677606,-1.39041198760718));
#18003=CARTESIAN_POINT('Ctrl Pts',(83.2310481942998,4.24902954905002,-1.27014888600867));
#18004=CARTESIAN_POINT('Ctrl Pts',(83.2367644142801,4.28365637951515,-1.14800097222107));
#18005=CARTESIAN_POINT('Ctrl Pts',(83.2424806342603,4.31300545590474,-1.02443786406786));
#18006=CARTESIAN_POINT('Ctrl Pts',(83.2481900066406,4.3423193743169,-0.901022775188253));
#18007=CARTESIAN_POINT('Ctrl Pts',(83.253899379021,4.36636802621654,-0.776196249202119));
#18008=CARTESIAN_POINT('Ctrl Pts',(83.2596087514013,4.38502115367675,-0.650444833792572));
#18009=CARTESIAN_POINT('Ctrl Pts',(83.2653126965135,4.40365654967427,-0.524812956328336));
#18010=CARTESIAN_POINT('Ctrl Pts',(83.2710166416257,4.41690656945924,-0.398258330848222));
#18011=CARTESIAN_POINT('Ctrl Pts',(83.276720586738,4.42469170305703,-0.271279068300975));
#18012=CARTESIAN_POINT('Ctrl Pts',(83.2824205200588,4.43247136108805,-0.144389114873869));
#18013=CARTESIAN_POINT('Ctrl Pts',(83.2881204533796,4.43479375906451,-0.0170755150908258));
#18014=CARTESIAN_POINT('Ctrl Pts',(83.2938203867003,4.43163111181196,0.110157563609088));
#18015=CARTESIAN_POINT('Ctrl Pts',(83.2995183245726,4.42846957174779,0.23734610019774));
#18016=CARTESIAN_POINT('Ctrl Pts',(83.3052162624448,4.41982681393095,0.364453774179399));
#18017=CARTESIAN_POINT('Ctrl Pts',(83.310914200317,4.4057271570083,0.490975781479656));
#18018=CARTESIAN_POINT('Ctrl Pts',(83.3166112906413,4.39162959735927,0.617478969083135));
#18019=CARTESIAN_POINT('Ctrl Pts',(83.3223083809656,4.37207679727301,0.743396267566183));
#18020=CARTESIAN_POINT('Ctrl Pts',(83.32800547129,4.34714496198324,0.868227896064));
#18021=CARTESIAN_POINT('Ctrl Pts',(83.3337029902522,4.32221125087115,0.993068916648394));
#18022=CARTESIAN_POINT('Ctrl Pts',(83.3394005092144,4.29189777752478,1.11682371416384));
#18023=CARTESIAN_POINT('Ctrl Pts',(83.3450980281766,4.25633179186417,1.23900309828763));
#18024=CARTESIAN_POINT('Ctrl Pts',(83.3507972519518,4.22075516414081,1.36121904095599));
#18025=CARTESIAN_POINT('Ctrl Pts',(83.3564964757269,4.17992300858298,1.48185825013476));
#18026=CARTESIAN_POINT('Ctrl Pts',(83.3621956995021,4.13401216616899,1.60044756551621));
#18027=CARTESIAN_POINT('Ctrl Pts',(83.3679010547031,4.08805193125264,1.71916446346274));
#18028=CARTESIAN_POINT('Ctrl Pts',(83.3736064099041,4.03700224421237,1.8358266926203));
#18029=CARTESIAN_POINT('Ctrl Pts',(83.3793117651051,3.98108787463452,1.94998162412829));
#18030=CARTESIAN_POINT('Ctrl Pts',(83.3850206254083,3.92513915389531,2.06420668706227));
#18031=CARTESIAN_POINT('Ctrl Pts',(83.3907294857114,3.86431998684683,2.17592103443391));
#18032=CARTESIAN_POINT('Ctrl Pts',(83.3964383460145,3.79890005935971,2.28469852256196));
#18033=CARTESIAN_POINT('Ctrl Pts',(83.4021554039637,3.73338619203564,2.39363220987718));
#18034=CARTESIAN_POINT('Ctrl Pts',(83.4078724619128,3.66325859195248,2.49962028578032));
#18035=CARTESIAN_POINT('Ctrl Pts',(83.4135895198619,3.58882923436517,2.60226703598342));
#18036=CARTESIAN_POINT('Ctrl Pts',(83.4160312917253,3.55704024205838,2.64610775768649));
#18037=CARTESIAN_POINT('Ctrl Pts',(83.4184730635886,3.52446702502304,2.68933939325408));
#18038=CARTESIAN_POINT('Ctrl Pts',(83.4209148354519,3.49113598849276,2.7319331085974));
#18039=CARTESIAN_POINT('Ctrl Pts',(83.4266198983286,3.41325989285673,2.83145093326986));
#18040=CARTESIAN_POINT('Ctrl Pts',(83.4323249612053,3.33100226602438,2.92779324457393));
#18041=CARTESIAN_POINT('Ctrl Pts',(83.438030024082,3.24465148343176,3.0205505708503));
#18042=CARTESIAN_POINT('Ctrl Pts',(83.4437280321523,3.15840748109027,3.11319319462721));
#18043=CARTESIAN_POINT('Ctrl Pts',(83.4494260402227,3.06808066251407,3.2022593622306));
#18044=CARTESIAN_POINT('Ctrl Pts',(83.455124048293,2.97400091869034,3.28737091543212));
#18045=CARTESIAN_POINT('Ctrl Pts',(83.4608164367597,2.88001396007733,3.37239852821163));
#18046=CARTESIAN_POINT('Ctrl Pts',(83.4665088252263,2.78228173585553,3.45347902008985));
#18047=CARTESIAN_POINT('Ctrl Pts',(83.4722012136929,2.6811720661167,3.53026986955325));
#18048=CARTESIAN_POINT('Ctrl Pts',(83.477889412659,2.58013681136487,3.60700420226529));
#18049=CARTESIAN_POINT('Ctrl Pts',(83.4835776116252,2.47572937575758,3.67945493462437));
#18050=CARTESIAN_POINT('Ctrl Pts',(83.4892658105913,2.3683514681524,3.74731908479921));
#18051=CARTESIAN_POINT('Ctrl Pts',(83.4949517923112,2.26101541619517,3.81515678169291));
#18052=CARTESIAN_POINT('Ctrl Pts',(83.5006377740312,2.15071153226204,3.87841123787996));
#18053=CARTESIAN_POINT('Ctrl Pts',(83.5063237557511,2.03787109472943,3.93682237359857));
#18054=CARTESIAN_POINT('Ctrl Pts',(83.5120087552445,1.92505014985086,3.99522341906863));
#18055=CARTESIAN_POINT('Ctrl Pts',(83.5176937547379,1.80969387814875,4.04878262428713));
#18056=CARTESIAN_POINT('Ctrl Pts',(83.5233787542313,1.69225830281663,4.09728578897642));
#18057=CARTESIAN_POINT('Ctrl Pts',(83.5290640603275,1.57481639396105,4.14579156953345));
#18058=CARTESIAN_POINT('Ctrl Pts',(83.5347493664237,1.45529532835186,4.1892406145228));
#18059=CARTESIAN_POINT('Ctrl Pts',(83.5404346725199,1.33417075941755,4.22746701757863));
#18060=CARTESIAN_POINT('Ctrl Pts',(83.5461215739581,1.21301220196906,4.26570414726618));
#18061=CARTESIAN_POINT('Ctrl Pts',(83.5518084753962,1.09024962761543,4.29871559940692));
#18062=CARTESIAN_POINT('Ctrl Pts',(83.5574953768344,0.966372968624036,4.32638559140453));
#18063=CARTESIAN_POINT('Ctrl Pts',(83.5631883104399,0.842364912113645,4.35408493330816));
#18064=CARTESIAN_POINT('Ctrl Pts',(83.5688812440455,0.717240802444245,4.37643141553077));
#18065=CARTESIAN_POINT('Ctrl Pts',(83.574574177651,0.591500159325903,4.39336050894044));
#18066=CARTESIAN_POINT('Ctrl Pts',(83.5802705426044,0.465683727534138,4.41029980615933));
#18067=CARTESIAN_POINT('Ctrl Pts',(83.5859669075578,0.33925041991595,4.42181517388166));
#18068=CARTESIAN_POINT('Ctrl Pts',(83.5916632725112,0.212702699705993,4.42789414524984));
#18069=CARTESIAN_POINT('Ctrl Pts',(83.5973678301151,0.0859729754876457,
4.43398185954245));
#18070=CARTESIAN_POINT('Ctrl Pts',(83.6030723877191,-0.0408710906136837,
4.43461756341891));
#18071=CARTESIAN_POINT('Ctrl Pts',(83.6087769453231,-0.167328842256537,
4.4298408615377));
#18072=CARTESIAN_POINT('Ctrl Pts',(83.6113505290768,-0.224379649305718,
4.4276858754351));
#18073=CARTESIAN_POINT('Ctrl Pts',(83.6139241128306,-0.281351919387955,
4.42442999190873));
#18074=CARTESIAN_POINT('Ctrl Pts',(83.6164976965844,-0.338200276830494,
4.420080267682));
#18075=CARTESIAN_POINT('Ctrl Pts',(83.6222109841139,-0.464402119368476,
4.4104239955109));
#18076=CARTESIAN_POINT('Ctrl Pts',(83.6279242716434,-0.590383458300955,
4.39534367157767));
#18077=CARTESIAN_POINT('Ctrl Pts',(83.6336375591729,-0.715642314386609,
4.37485372073849));
#18078=CARTESIAN_POINT('Ctrl Pts',(83.6393439004404,-0.840748879722081,
4.3543886817505));
#18079=CARTESIAN_POINT('Ctrl Pts',(83.6450502417078,-0.965134319568548,
4.32852716489467));
#18080=CARTESIAN_POINT('Ctrl Pts',(83.6507565829752,-1.08829986702525,4.29733549998517));
#18081=CARTESIAN_POINT('Ctrl Pts',(83.6564574025489,-1.21134623436123,4.26617401743159));
#18082=CARTESIAN_POINT('Ctrl Pts',(83.6621582221225,-1.3331746737723,4.22969274740485));
#18083=CARTESIAN_POINT('Ctrl Pts',(83.6678590416961,-1.45329519728146,4.18800932061506));
#18084=CARTESIAN_POINT('Ctrl Pts',(83.6735557591892,-1.5733292868919,4.14635588754312));
#18085=CARTESIAN_POINT('Ctrl Pts',(83.6792524766823,-1.6916575311311,4.09950787836922));
#18086=CARTESIAN_POINT('Ctrl Pts',(83.6849491941753,-1.80780418804368,4.04763301420617));
#18087=CARTESIAN_POINT('Ctrl Pts',(83.6906437933859,-1.92390765667619,3.9957774393298));
#18088=CARTESIAN_POINT('Ctrl Pts',(83.6963383925965,-2.03783078739654,3.93889888846478));
#18089=CARTESIAN_POINT('Ctrl Pts',(83.7020329918071,-2.14911725028655,3.87721343809195));
#18090=CARTESIAN_POINT('Ctrl Pts',(83.7077266679151,-2.26038567348426,3.81553798701746));
#18091=CARTESIAN_POINT('Ctrl Pts',(83.7134203440232,-2.36901793033941,3.74905737964579));
#18092=CARTESIAN_POINT('Ctrl Pts',(83.7191140201312,-2.47458224161525,3.67803367704572));
#18093=CARTESIAN_POINT('Ctrl Pts',(83.7248080528019,-2.58015316378562,3.60700552663368));
#18094=CARTESIAN_POINT('Ctrl Pts',(83.7305020854726,-2.68265542734863,3.53143393775299));
#18095=CARTESIAN_POINT('Ctrl Pts',(83.7361961181433,-2.78168662765078,3.45162403884734));
#18096=CARTESIAN_POINT('Ctrl Pts',(83.7418917869822,-2.88074628435806,3.37179120673671));
#18097=CARTESIAN_POINT('Ctrl Pts',(83.7475874558211,-2.97633258319261,3.28771789193997));
#18098=CARTESIAN_POINT('Ctrl Pts',(83.75328312466,-3.06807696429394,3.19974885595243));
#18099=CARTESIAN_POINT('Ctrl Pts',(83.7589848401618,-3.15991874349887,3.11168642986101));
#18100=CARTESIAN_POINT('Ctrl Pts',(83.7646865556636,-3.24791017329906,3.0197203012298));
#18101=CARTESIAN_POINT('Ctrl Pts',(83.7703882711653,-3.33172006525766,2.92423159253153));
#18102=CARTESIAN_POINT('Ctrl Pts',(83.7760934383249,-3.41558069336201,2.8286850776611));
#18103=CARTESIAN_POINT('Ctrl Pts',(83.7817986054845,-3.49525449117515,2.72961204476918));
#18104=CARTESIAN_POINT('Ctrl Pts',(83.7875037726441,-3.57045198052145,2.6274249094485));
#18105=CARTESIAN_POINT('Ctrl Pts',(83.7932170873008,-3.6457568587145,2.52509184161452));
#18106=CARTESIAN_POINT('Ctrl Pts',(83.7989304019574,-3.71657244207957,2.41963612160936));
#18107=CARTESIAN_POINT('Ctrl Pts',(83.804643716614,-3.78265359926121,2.31149751200303));
#18108=CARTESIAN_POINT('Ctrl Pts',(83.8071226636483,-3.81132551713363,2.26457730863935));
#18109=CARTESIAN_POINT('Ctrl Pts',(83.8096016106825,-3.83910672862993,2.21715231825351));
#18110=CARTESIAN_POINT('Ctrl Pts',(83.8120805577167,-3.8659800018218,2.16925969526793));
#18111=CARTESIAN_POINT('Ctrl Pts',(83.8180254810596,-3.93042653774616,2.05440529603959));
#18112=CARTESIAN_POINT('Ctrl Pts',(83.8239704044024,-3.98983198688334,1.93653249703956));
#18113=CARTESIAN_POINT('Ctrl Pts',(83.8299153277452,-4.04391631419735,1.81610292763614));
#18114=CARTESIAN_POINT('Ctrl Pts',(83.8358508814789,-4.09791540088159,1.69586316353951));
#18115=CARTESIAN_POINT('Ctrl Pts',(83.8417864352125,-4.14660992797813,1.57307497537607));
#18116=CARTESIAN_POINT('Ctrl Pts',(83.8477219889461,-4.18976514839525,1.44822546631817));
#18117=CARTESIAN_POINT('Ctrl Pts',(83.853645865327,-4.23283546708994,1.32362158080853));
#18118=CARTESIAN_POINT('Ctrl Pts',(83.8595697417078,-4.27038809194831,1.19696479106409));
#18119=CARTESIAN_POINT('Ctrl Pts',(83.8654936180886,-4.30223616830599,1.06876234594966));
#18120=CARTESIAN_POINT('Ctrl Pts',(83.8714105761186,-4.33404705007198,0.940709625344368));
#18121=CARTESIAN_POINT('Ctrl Pts',(83.8773275341486,-4.36016656697666,0.811115184524049));
#18122=CARTESIAN_POINT('Ctrl Pts',(83.8832444921787,-4.38045717906978,0.680502683562672));
#18123=CARTESIAN_POINT('Ctrl Pts',(83.8891531086527,-4.40071918604579,0.550074316321375));
#18124=CARTESIAN_POINT('Ctrl Pts',(83.8950617251268,-4.41516861656605,0.418631097111072));
#18125=CARTESIAN_POINT('Ctrl Pts',(83.9009703416008,-4.42371876807926,0.286707622750609));
#18126=CARTESIAN_POINT('Ctrl Pts',(83.9052496078144,-4.42991114401917,0.191163146459511));
#18127=CARTESIAN_POINT('Ctrl Pts',(83.9095288740281,-4.43301023979327,0.095367055746549));
#18128=CARTESIAN_POINT('Ctrl Pts',(83.9138081402417,-4.43299997457307,-0.000474800080565356));
#18129=CARTESIAN_POINT('',(85.1638081402016,-4.43299950255766,-0.00210007702333454));
#18130=CARTESIAN_POINT('Ctrl Pts',(83.91380814028,-4.43299997457298,-0.000474800938941129));
#18131=CARTESIAN_POINT('Ctrl Pts',(83.9198146375964,-4.43298556599779,-0.135001100795744));
#18132=CARTESIAN_POINT('Ctrl Pts',(83.9258211349128,-4.42684326063918,-0.269394591604568));
#18133=CARTESIAN_POINT('Ctrl Pts',(83.9318276322292,-4.4146348479927,-0.403098200056139));
#18134=CARTESIAN_POINT('Ctrl Pts',(83.9381472811142,-4.4017899439988,-0.543772509151691));
#18135=CARTESIAN_POINT('Ctrl Pts',(83.9444669299992,-4.38222954173958,-0.683682637169625));
#18136=CARTESIAN_POINT('Ctrl Pts',(83.9507865788842,-4.35608620402984,-0.822193397602375));
#18137=CARTESIAN_POINT('Ctrl Pts',(83.9568184974464,-4.33113315887183,-0.95439783524233));
#18138=CARTESIAN_POINT('Ctrl Pts',(83.9628504160087,-4.30018351207985,-1.08532723336189));
#18139=CARTESIAN_POINT('Ctrl Pts',(83.9688823345709,-4.26340353906825,-1.21444607252044));
#18140=CARTESIAN_POINT('Ctrl Pts',(83.9749228194931,-4.22657133218006,-1.34374828259957));
#18141=CARTESIAN_POINT('Ctrl Pts',(83.9809633044154,-4.18389237439995,-1.47123449090566));
#18142=CARTESIAN_POINT('Ctrl Pts',(83.9870037893376,-4.13558151938089,-1.59638795302246));
#18143=CARTESIAN_POINT('Ctrl Pts',(83.9930571147078,-4.08716796846467,-1.72180745777232));
#18144=CARTESIAN_POINT('Ctrl Pts',(83.9991104400779,-4.033098721031,-1.84488400437242));
#18145=CARTESIAN_POINT('Ctrl Pts',(84.0051637654481,-3.97363566494557,-1.96512305016062));
#18146=CARTESIAN_POINT('Ctrl Pts',(84.0059969832484,-3.96545079567714,-1.98167350914348));
#18147=CARTESIAN_POINT('Ctrl Pts',(84.0068302010488,-3.95716380076966,-1.99817025067915));
#18148=CARTESIAN_POINT('Ctrl Pts',(84.0076634188491,-3.94877542780791,-2.01461202734929));
#18149=CARTESIAN_POINT('Ctrl Pts',(84.0133739097053,-3.89128538489826,-2.12729638826019));
#18150=CARTESIAN_POINT('Ctrl Pts',(84.0190844005613,-3.82887916097553,-2.23769221763686));
#18151=CARTESIAN_POINT('Ctrl Pts',(84.0247948914174,-3.76176283356058,-2.34534206120179));
#18152=CARTESIAN_POINT('Ctrl Pts',(84.0304984050993,-3.6947285100087,-2.45286037636863));
#18153=CARTESIAN_POINT('Ctrl Pts',(84.0362019187812,-3.62299574155127,-2.55763904467317));
#18154=CARTESIAN_POINT('Ctrl Pts',(84.0419054324631,-3.54681729055957,-2.65924352164063));
#18155=CARTESIAN_POINT('Ctrl Pts',(84.0476033971757,-3.47071295385949,-2.76074914724346));
#18156=CARTESIAN_POINT('Ctrl Pts',(84.0533013618884,-3.39017177929827,-2.85908640886412));
#18157=CARTESIAN_POINT('Ctrl Pts',(84.0589993266011,-3.30549051446267,-2.95384858427058));
#18158=CARTESIAN_POINT('Ctrl Pts',(84.0646931655529,-3.22087056531951,-3.04854214463671));
#18159=CARTESIAN_POINT('Ctrl Pts',(84.0703870045047,-3.13211675741254,-3.13966547422476));
#18160=CARTESIAN_POINT('Ctrl Pts',(84.0760808434565,-3.03956660109192,-3.22684425988093));
#18161=CARTESIAN_POINT('Ctrl Pts',(84.0817725395899,-2.94705127508153,-3.3139902366876));
#18162=CARTESIAN_POINT('Ctrl Pts',(84.0874642357232,-2.85074273159858,-3.39719434791402));
#18163=CARTESIAN_POINT('Ctrl Pts',(84.0931559318566,-2.75101565081883,-3.47611879672572));
#18164=CARTESIAN_POINT('Ctrl Pts',(84.0988466905102,-2.65130499609671,-3.55503024588341));
#18165=CARTESIAN_POINT('Ctrl Pts',(84.1045374491637,-2.54817723703542,-3.62966318704529));
#18166=CARTESIAN_POINT('Ctrl Pts',(84.1102282078173,-2.44204005555012,-3.69972017416031));
#18167=CARTESIAN_POINT('Ctrl Pts',(84.1159193118143,-2.33589643313382,-3.76978141268103));
#18168=CARTESIAN_POINT('Ctrl Pts',(84.1216104158113,-2.22674335831257,-3.83526592490555));
#18169=CARTESIAN_POINT('Ctrl Pts',(84.1273015198083,-2.1150169611824,-3.89591994962817));
#18170=CARTESIAN_POINT('Ctrl Pts',(84.1329942519059,-2.00325860156997,-3.95659132614266));
#18171=CARTESIAN_POINT('Ctrl Pts',(84.1386869840035,-1.88892580592011,-4.01242927568396));
#18172=CARTESIAN_POINT('Ctrl Pts',(84.1443797161011,-1.77247825695833,-4.06322652932494));
#18173=CARTESIAN_POINT('Ctrl Pts',(84.1500784986159,-1.65590694382871,-4.11407777190669));
#18174=CARTESIAN_POINT('Ctrl Pts',(84.1557772811306,-1.53721675604236,-4.15987746213883));
#18175=CARTESIAN_POINT('Ctrl Pts',(84.1614760636454,-1.41688654766952,-4.20046682060853));
#18176=CARTESIAN_POINT('Ctrl Pts',(84.167178296002,-1.2964834956349,-4.24108075044348));
#18177=CARTESIAN_POINT('Ctrl Pts',(84.1728805283586,-1.17443882806854,-4.27647795407286));
#18178=CARTESIAN_POINT('Ctrl Pts',(84.1785827607152,-1.05124421479158,-4.3065501971842));
#18179=CARTESIAN_POINT('Ctrl Pts',(84.184293163262,-0.927873087587349,-4.33666552797276));
#18180=CARTESIAN_POINT('Ctrl Pts',(84.1900035658089,-0.803349115433806,
-4.36144058594429));
#18181=CARTESIAN_POINT('Ctrl Pts',(84.1957139683557,-0.678172125810452,
-4.38081859562499));
#18182=CARTESIAN_POINT('Ctrl Pts',(84.1982247388976,-0.623133852152641,
-4.38933878933599));
#18183=CARTESIAN_POINT('Ctrl Pts',(84.2007355094395,-0.567969378517666,
-4.39681629432521));
#18184=CARTESIAN_POINT('Ctrl Pts',(84.2032462799814,-0.512721254578061,
-4.40324947227657));
#18185=CARTESIAN_POINT('Ctrl Pts',(84.208957745036,-0.387043609430515,-4.41788357381866));
#18186=CARTESIAN_POINT('Ctrl Pts',(84.2146692100905,-0.26054526117373,-4.42715530760686));
#18187=CARTESIAN_POINT('Ctrl Pts',(84.2203806751451,-0.133721359890292,
-4.43098268986791));
#18188=CARTESIAN_POINT('Ctrl Pts',(84.2260851767589,-0.00705208280799532,
-4.4348054057694));
#18189=CARTESIAN_POINT('Ctrl Pts',(84.2317896783727,0.119941562127036,-4.43319696397356));
#18190=CARTESIAN_POINT('Ctrl Pts',(84.2374941799866,0.246757627535567,-4.42612693822184));
#18191=CARTESIAN_POINT('Ctrl Pts',(84.2431931450881,0.373450611428637,-4.41906377429382));
#18192=CARTESIAN_POINT('Ctrl Pts',(84.2488921101896,0.499965962500836,-4.40654959625833));
#18193=CARTESIAN_POINT('Ctrl Pts',(84.2545910752912,0.625800519172279,-4.38860600990835));
#18194=CARTESIAN_POINT('Ctrl Pts',(84.2602859258295,0.751544225271094,-4.37067537854577));
#18195=CARTESIAN_POINT('Ctrl Pts',(84.2659807763678,0.876607721485549,-4.34732319692061));
#18196=CARTESIAN_POINT('Ctrl Pts',(84.271675626906,1.00049223376467,-4.318622962262));
#18197=CARTESIAN_POINT('Ctrl Pts',(84.2773683475706,1.12433041324489,-4.28993346148913));
#18198=CARTESIAN_POINT('Ctrl Pts',(84.2830610682352,1.24699009734483,-4.25589997462425));
#18199=CARTESIAN_POINT('Ctrl Pts',(84.2887537888998,1.36798230660267,-4.21664717623161));
#18200=CARTESIAN_POINT('Ctrl Pts',(84.2944455798391,1.48895475562298,-4.17740078853786));
#18201=CARTESIAN_POINT('Ctrl Pts',(84.3001373707785,1.6082598919955,-4.13293690795331));
#18202=CARTESIAN_POINT('Ctrl Pts',(84.3058291617178,1.72542403151994,-4.08343004243411));
#18203=CARTESIAN_POINT('Ctrl Pts',(84.3115213046565,1.84259541686544,-4.03392011524528));
#18204=CARTESIAN_POINT('Ctrl Pts',(84.3172134475951,1.95762517436972,-3.97936673818128));
#18205=CARTESIAN_POINT('Ctrl Pts',(84.3229055905338,2.07006021194999,-3.91999231107684));
#18206=CARTESIAN_POINT('Ctrl Pts',(84.3285993671343,2.18252751871783,-3.86060084333661));
#18207=CARTESIAN_POINT('Ctrl Pts',(84.3342931437348,2.2923982713242,-3.79638575927441));
#18208=CARTESIAN_POINT('Ctrl Pts',(84.3399869203353,2.39924501807703,-3.72761483300415));
#18209=CARTESIAN_POINT('Ctrl Pts',(84.3456867501181,2.50620535601741,-3.6587707948103));
#18210=CARTESIAN_POINT('Ctrl Pts',(84.351386579901,2.61013493331779,-3.58536146017421));
#18211=CARTESIAN_POINT('Ctrl Pts',(84.3570864096839,2.71063602804441,-3.50769743898582));
#18212=CARTESIAN_POINT('Ctrl Pts',(84.3627896923141,2.81119800440306,-3.42998637042571));
#18213=CARTESIAN_POINT('Ctrl Pts',(84.3684929749443,2.90832705621915,-3.34801573778199));
#18214=CARTESIAN_POINT('Ctrl Pts',(84.3741962575746,3.00166042348645,-3.26213483811984));
#18215=CARTESIAN_POINT('Ctrl Pts',(84.3799077059024,3.09512742117307,-3.17613097813847));
#18216=CARTESIAN_POINT('Ctrl Pts',(84.3856191542302,3.18478760174866,-3.08620595416674));
#18217=CARTESIAN_POINT('Ctrl Pts',(84.391330602558,3.27031650948386,-2.99274438063082));
#18218=CARTESIAN_POINT('Ctrl Pts',(84.3938301154099,3.30774670088692,-2.95184260041503));
#18219=CARTESIAN_POINT('Ctrl Pts',(84.3963296282619,3.3443862002125,-2.91026390191573));
#18220=CARTESIAN_POINT('Ctrl Pts',(84.3988291411138,3.38021038982991,-2.86804231497478));
#18221=CARTESIAN_POINT('Ctrl Pts',(84.4045403172651,3.46206564303368,-2.77156954820392));
#18222=CARTESIAN_POINT('Ctrl Pts',(84.4102514934165,3.5399137973655,-2.67144091763106));
#18223=CARTESIAN_POINT('Ctrl Pts',(84.4159626695678,3.61341209461349,-2.56802298169252));
#18224=CARTESIAN_POINT('Ctrl Pts',(84.4216668798357,3.6868207464796,-2.46473118391919));
#18225=CARTESIAN_POINT('Ctrl Pts',(84.4273710901036,3.7558898671908,-2.35815838504291));
#18226=CARTESIAN_POINT('Ctrl Pts',(84.4330753003716,3.82031583393719,-2.24870538954501));
#18227=CARTESIAN_POINT('Ctrl Pts',(84.4387739720551,3.8846792453711,-2.1393586689962));
#18228=CARTESIAN_POINT('Ctrl Pts',(84.4444726437386,3.94440827244869,-2.02713765864749));
#18229=CARTESIAN_POINT('Ctrl Pts',(84.4501713154221,3.99924191897012,-1.91247302557505));
#18230=CARTESIAN_POINT('Ctrl Pts',(84.455865870837,4.05403595801321,-1.79789121714149));
#18231=CARTESIAN_POINT('Ctrl Pts',(84.461560426252,4.10394148266522,-1.68086965789851));
#18232=CARTESIAN_POINT('Ctrl Pts',(84.4672549816669,4.14874311284873,-1.56186413736607));
#18233=CARTESIAN_POINT('Ctrl Pts',(84.4729474057725,4.19352797506243,-1.44290315719891));
#18234=CARTESIAN_POINT('Ctrl Pts',(84.4786398298781,4.23321260059651,-1.32196006511392));
#18235=CARTESIAN_POINT('Ctrl Pts',(84.4843322539837,4.26762962970939,-1.19951087682708));
#18236=CARTESIAN_POINT('Ctrl Pts',(84.4900237475625,4.30204103275377,-1.07708170501287));
#18237=CARTESIAN_POINT('Ctrl Pts',(84.4957152411413,4.33118644417461,-0.953147310833609));
#18238=CARTESIAN_POINT('Ctrl Pts',(84.5014067347201,4.35494845637367,-0.828198612851177));
#18239=CARTESIAN_POINT('Ctrl Pts',(84.5070985798207,4.37871193617777,-0.703242197704976));
#18240=CARTESIAN_POINT('Ctrl Pts',(84.5127904249213,4.39709128089044,-0.577271746302338));
#18241=CARTESIAN_POINT('Ctrl Pts',(84.5184822700218,4.41002035645222,-0.450787594857083));
#18242=CARTESIAN_POINT('Ctrl Pts',(84.5241757486305,4.42295314254171,-0.324267143604716));
#18243=CARTESIAN_POINT('Ctrl Pts',(84.5298692272391,4.43043250721369,-0.197233095956277));
#18244=CARTESIAN_POINT('Ctrl Pts',(84.5355627058477,4.43244429394526,-0.0701896080064969));
#18245=CARTESIAN_POINT('Ctrl Pts',(84.541262239029,4.43445822005588,0.0569889808327634));
#18246=CARTESIAN_POINT('Ctrl Pts',(84.5469617722102,4.4309929529109,0.184176630558526));
#18247=CARTESIAN_POINT('Ctrl Pts',(84.5526613053914,4.42208646834404,0.31087017626094));
#18248=CARTESIAN_POINT('Ctrl Pts',(84.5583642918138,4.41317458750389,0.437640483225464));
#18249=CARTESIAN_POINT('Ctrl Pts',(84.5640672782362,4.39881496678714,0.563915693839469));
#18250=CARTESIAN_POINT('Ctrl Pts',(84.5697702646585,4.37909716271554,0.689200289826353));
#18251=CARTESIAN_POINT('Ctrl Pts',(84.5754814199594,4.35935111513531,0.814664341728014));
#18252=CARTESIAN_POINT('Ctrl Pts',(84.5811925752603,4.33423163784856,0.939134555313065));
#18253=CARTESIAN_POINT('Ctrl Pts',(84.5869037305611,4.30387891674065,1.06212770891042));
#18254=CARTESIAN_POINT('Ctrl Pts',(84.5894064877895,4.29057766889308,1.11602608638165));
#18255=CARTESIAN_POINT('Ctrl Pts',(84.5919092450178,4.27627207253842,1.16964103157631));
#18256=CARTESIAN_POINT('Ctrl Pts',(84.5944120022462,4.26097685905561,1.22293303438601));
#18257=CARTESIAN_POINT('Ctrl Pts',(84.6001231015456,4.22607435951755,1.34454128166795));
#18258=CARTESIAN_POINT('Ctrl Pts',(84.6058342008451,4.18590781848005,1.46484180421131));
#18259=CARTESIAN_POINT('Ctrl Pts',(84.6115453001445,4.140592234111,1.58334612476858));
#18260=CARTESIAN_POINT('Ctrl Pts',(84.617249431588,4.09533193725281,1.70170586352247));
#18261=CARTESIAN_POINT('Ctrl Pts',(84.6229535630315,4.04493523656118,1.818273390522));
#18262=CARTESIAN_POINT('Ctrl Pts',(84.6286576944749,3.98956732935321,1.93257380830785));
#18263=CARTESIAN_POINT('Ctrl Pts',(84.634356285467,3.93425320127051,2.04676320552606));
#18264=CARTESIAN_POINT('Ctrl Pts',(84.6400548764591,3.87397764784127,2.15868951808578));
#18265=CARTESIAN_POINT('Ctrl Pts',(84.6457534674512,3.80895435337528,2.26789676438402));
#18266=CARTESIAN_POINT('Ctrl Pts',(84.6514479404111,3.74397804736939,2.37702509311312));
#18267=CARTESIAN_POINT('Ctrl Pts',(84.657142413371,3.6742610323866,2.48343792453169));
#18268=CARTESIAN_POINT('Ctrl Pts',(84.662836886331,3.60006319251113,2.58670330921939));
#18269=CARTESIAN_POINT('Ctrl Pts',(84.6685292256521,3.5258931535212,2.68993000182194));
#18270=CARTESIAN_POINT('Ctrl Pts',(84.6742215649733,3.44724586040078,2.79001126890387));
#18271=CARTESIAN_POINT('Ctrl Pts',(84.6799139042944,3.36442465521006,2.88654390914371));
#18272=CARTESIAN_POINT('Ctrl Pts',(84.6856053116618,3.28161700956417,2.98306074499313));
#18273=CARTESIAN_POINT('Ctrl Pts',(84.6912967190292,3.19463707092638,3.07602980678651));
#18274=CARTESIAN_POINT('Ctrl Pts',(84.6969881263966,3.10382828035472,3.16508120054925));
#18275=CARTESIAN_POINT('Ctrl Pts',(84.7026798839471,3.0130139024665,3.25413807349878));
#18276=CARTESIAN_POINT('Ctrl Pts',(84.7083716414975,2.91837048910615,3.33927651950545));
#18277=CARTESIAN_POINT('Ctrl Pts',(84.7140633990479,2.82027774807047,3.42016409310117));
#18278=CARTESIAN_POINT('Ctrl Pts',(84.7197567888548,2.72215687644153,3.50107486326993));
#18279=CARTESIAN_POINT('Ctrl Pts',(84.7254501786618,2.62058501715931,3.57773208207322));
#18280=CARTESIAN_POINT('Ctrl Pts',(84.7311435684687,2.5159738764591,3.64984444229824));
#18281=CARTESIAN_POINT('Ctrl Pts',(84.7368430114296,2.41125151426046,3.72203347164957));
#18282=CARTESIAN_POINT('Ctrl Pts',(84.7425424543906,2.30348374786703,3.78966776794911));
#18283=CARTESIAN_POINT('Ctrl Pts',(84.7482418973515,2.1931103637717,3.85249995876926));
#18284=CARTESIAN_POINT('Ctrl Pts',(84.7539447926189,2.08267012353876,3.91537020874317));
#18285=CARTESIAN_POINT('Ctrl Pts',(84.7596476878863,1.96962147595197,3.97343237656758));
#18286=CARTESIAN_POINT('Ctrl Pts',(84.7653505831536,1.85442644308312,4.02648625568175));
#18287=CARTESIAN_POINT('Ctrl Pts',(84.7710616466507,1.73906641691927,4.07961612361341));
#18288=CARTESIAN_POINT('Ctrl Pts',(84.7767727101477,1.62155423549691,4.12772322845963));
#18289=CARTESIAN_POINT('Ctrl Pts',(84.7824837736447,1.50236975911596,4.1706563160843));
#18290=CARTESIAN_POINT('Ctrl Pts',(84.7849874702226,1.45011998710461,4.18947792866547));
#18291=CARTESIAN_POINT('Ctrl Pts',(84.7874911668006,1.39754898808281,4.20730580431343));
#18292=CARTESIAN_POINT('Ctrl Pts',(84.7899948633785,1.34469785821158,4.22413028564712));
#18293=CARTESIAN_POINT('Ctrl Pts',(84.7957060737223,1.22413855311901,4.26250879870963));
#18294=CARTESIAN_POINT('Ctrl Pts',(84.8014172840661,1.10174897916768,4.29578114366027));
#18295=CARTESIAN_POINT('Ctrl Pts',(84.8071284944099,0.977999442804644,4.32377220605732));
#18296=CARTESIAN_POINT('Ctrl Pts',(84.8128327385545,0.854400848862536,4.35172912659941));
#18297=CARTESIAN_POINT('Ctrl Pts',(84.8185369826992,0.729445978649419,4.37441749312619));
#18298=CARTESIAN_POINT('Ctrl Pts',(84.8242412268438,0.603621667297139,4.39171149812569));
#18299=CARTESIAN_POINT('Ctrl Pts',(84.8299399320477,0.47791953399142,4.40898871028346));
#18300=CARTESIAN_POINT('Ctrl Pts',(84.8356386372515,0.35135003268023,4.42088192981958));
#18301=CARTESIAN_POINT('Ctrl Pts',(84.8413373424554,0.224411137252003,4.42731618946256));
#18302=CARTESIAN_POINT('Ctrl Pts',(84.8470319309937,0.0975639407203271,
4.43374580108566));
#18303=CARTESIAN_POINT('Ctrl Pts',(84.852726519532,-0.0296517215462163,
4.43472428139404));
#18304=CARTESIAN_POINT('Ctrl Pts',(84.8584211080703,-0.156732262753133,
4.43022843630126));
#18305=CARTESIAN_POINT('Ctrl Pts',(84.8641135645791,-0.283765225549177,
4.42573427443364));
#18306=CARTESIAN_POINT('Ctrl Pts',(84.8698060210878,-0.410662769618349,
4.41576987647275));
#18307=CARTESIAN_POINT('Ctrl Pts',(84.8754984775965,-0.536921139781867,
4.40036415420989));
#18308=CARTESIAN_POINT('Ctrl Pts',(84.8811900031187,-0.663158860714335,
4.38496095151321));
#18309=CARTESIAN_POINT('Ctrl Pts',(84.8868815286408,-0.788757219601314,
4.36411824296008));
#18310=CARTESIAN_POINT('Ctrl Pts',(84.8925730541629,-0.913217949425142,
4.33791677846034));
#18311=CARTESIAN_POINT('Ctrl Pts',(84.8982649307097,-1.03768635535937,4.31171369798635));
#18312=CARTESIAN_POINT('Ctrl Pts',(84.9039568072564,-1.16101660207895,4.28015128646399));
#18313=CARTESIAN_POINT('Ctrl Pts',(84.9096486838031,-1.28272148158459,4.24336123853266));
#18314=CARTESIAN_POINT('Ctrl Pts',(84.915342193323,-1.40446127765892,4.20656063570624));
#18315=CARTESIAN_POINT('Ctrl Pts',(84.9210357028429,-1.52457439694119,4.16452952832993));
#18316=CARTESIAN_POINT('Ctrl Pts',(84.9267292123628,-1.64259012738771,4.11744904927899));
#18317=CARTESIAN_POINT('Ctrl Pts',(84.9324287754738,-1.76073133737822,4.07031851218053));
#18318=CARTESIAN_POINT('Ctrl Pts',(84.9381283385848,-1.87677033494921,4.01812803219668));
#18319=CARTESIAN_POINT('Ctrl Pts',(84.9438279016958,-1.99025740351014,3.9611064701385));
#18320=CARTESIAN_POINT('Ctrl Pts',(84.9495309175265,-2.10381322103226,3.90405036517419));
#18321=CARTESIAN_POINT('Ctrl Pts',(84.9552339333572,-2.21481368183004,3.84215754205619));
#18322=CARTESIAN_POINT('Ctrl Pts',(84.960936949188,-2.3228359939973,3.77570151693571));
#18323=CARTESIAN_POINT('Ctrl Pts',(84.9666481328379,-2.43101301496091,3.70915031396307));
#18324=CARTESIAN_POINT('Ctrl Pts',(84.9723593164879,-2.53620304061023,3.63802308244691));
#18325=CARTESIAN_POINT('Ctrl Pts',(84.9780705001378,-2.63801412851126,3.5626353248368));
#18326=CARTESIAN_POINT('Ctrl Pts',(84.9805729082622,-2.68262360163107,3.52960347913115));
#18327=CARTESIAN_POINT('Ctrl Pts',(84.9830753163866,-2.7265848239857,3.49575418657852));
#18328=CARTESIAN_POINT('Ctrl Pts',(84.9855777245109,-2.76986702128935,3.4611162483184));
#18329=CARTESIAN_POINT('Ctrl Pts',(84.9912243167992,-2.86753171440395,3.38295700916141));
#18330=CARTESIAN_POINT('Ctrl Pts',(84.9968709090875,-2.96205339025877,3.30052625266452));
#18331=CARTESIAN_POINT('Ctrl Pts',(85.0025175013757,-3.053030434426,3.21410861149224));
#18332=CARTESIAN_POINT('Ctrl Pts',(85.0081571642047,-3.1438958321889,3.12779702145622));
#18333=CARTESIAN_POINT('Ctrl Pts',(85.0137968270336,-3.23122495445217,3.03750855549499));
#18334=CARTESIAN_POINT('Ctrl Pts',(85.0194364898626,-3.31464763040675,2.94356927661621));
#18335=CARTESIAN_POINT('Ctrl Pts',(85.025070718161,-3.39798991803049,2.84972052014929));
#18336=CARTESIAN_POINT('Ctrl Pts',(85.0307049464594,-3.47743297650439,2.752228252434));
#18337=CARTESIAN_POINT('Ctrl Pts',(85.0363391747578,-3.55264247977328,2.65145628116143));
#18338=CARTESIAN_POINT('Ctrl Pts',(85.0419695096807,-3.6278000116239,2.55075394553382));
#18339=CARTESIAN_POINT('Ctrl Pts',(85.0475998446036,-3.69872956427739,2.44677674203878));
#18340=CARTESIAN_POINT('Ctrl Pts',(85.0532301795266,-3.76513660798485,2.33992207631201));
#18341=CARTESIAN_POINT('Ctrl Pts',(85.0588585031136,-3.83151992897065,2.23310558249219));
#18342=CARTESIAN_POINT('Ctrl Pts',(85.0644868267007,-3.89338373725461,2.12341401726423));
#18343=CARTESIAN_POINT('Ctrl Pts',(85.0701151502877,-3.9504767177598,2.01127390040187));
#18344=CARTESIAN_POINT('Ctrl Pts',(85.0757428051582,-4.00756291489102,1.89914710721509));
#18345=CARTESIAN_POINT('Ctrl Pts',(85.0813704600287,-4.05987922626133,1.78457270583772));
#18346=CARTESIAN_POINT('Ctrl Pts',(85.0869981148991,-4.10722052283786,1.66800137193573));
#18347=CARTESIAN_POINT('Ctrl Pts',(85.092626442901,-4.15456748197023,1.55141609478051));
#18348=CARTESIAN_POINT('Ctrl Pts',(85.0982547709027,-4.19693809021681,1.43283378979986));
#18349=CARTESIAN_POINT('Ctrl Pts',(85.1038830989045,-4.23417579195539,1.31272402385989));
#18350=CARTESIAN_POINT('Ctrl Pts',(85.1095163365026,-4.27144597617936,1.19250948604803));
#18351=CARTESIAN_POINT('Ctrl Pts',(85.1151495741007,-4.3035741926547,1.07076521833574));
#18352=CARTESIAN_POINT('Ctrl Pts',(85.1207828116988,-4.33045408028453,0.947974925062423));
#18353=CARTESIAN_POINT('Ctrl Pts',(85.1264187717764,-4.35734695865774,0.82512528863957));
#18354=CARTESIAN_POINT('Ctrl Pts',(85.132054731854,-4.37898638639673,0.701229022711327));
#18355=CARTESIAN_POINT('Ctrl Pts',(85.1376906919317,-4.39531760270183,0.576777401931996));
#18356=CARTESIAN_POINT('Ctrl Pts',(85.1433341965746,-4.41167068075284,0.452159184270924));
#18357=CARTESIAN_POINT('Ctrl Pts',(85.1489777012174,-4.42270132347423,0.326984534477598));
#18358=CARTESIAN_POINT('Ctrl Pts',(85.1546212058603,-4.42840682077849,0.201747440337038));
#18359=CARTESIAN_POINT('Ctrl Pts',(85.1576835173074,-4.43150277104552,0.133790556936706));
#18360=CARTESIAN_POINT('Ctrl Pts',(85.1607458287545,-4.43303167658465,0.0658152632455171));
#18361=CARTESIAN_POINT('Ctrl Pts',(85.1638081402016,-4.43299950255766,-0.00210007702333399));
#18362=CARTESIAN_POINT('',(86.4138081166213,-4.43234892329218,0.00349148966335142));
#18363=CARTESIAN_POINT('Ctrl Pts',(85.1638081402417,-4.43299950255724,-0.00210007791362036));
#18364=CARTESIAN_POINT('Ctrl Pts',(85.1695922887089,-4.43293873165559,-0.130379783652825));
#18365=CARTESIAN_POINT('Ctrl Pts',(85.1753764371761,-4.42731018443659,-0.258519691248014));
#18366=CARTESIAN_POINT('Ctrl Pts',(85.1811605856433,-4.4161479401985,-0.386168836495802));
#18367=CARTESIAN_POINT('Ctrl Pts',(85.186871750214,-4.40512654021482,-0.512207315617334));
#18368=CARTESIAN_POINT('Ctrl Pts',(85.1925829147847,-4.38868807156609,-0.637968011965168));
#18369=CARTESIAN_POINT('Ctrl Pts',(85.1982940793554,-4.36685208303201,-0.762949464197328));
#18370=CARTESIAN_POINT('Ctrl Pts',(85.2039982771344,-4.34504273123389,-0.887778457201997));
#18371=CARTESIAN_POINT('Ctrl Pts',(85.2097024749135,-4.31784902678548,-1.01182970738669));
#18372=CARTESIAN_POINT('Ctrl Pts',(85.2154066726925,-4.28534238745932,-1.1346054918977));
#18373=CARTESIAN_POINT('Ctrl Pts',(85.2211053309981,-4.25286731605446,-1.25726204611044));
#18374=CARTESIAN_POINT('Ctrl Pts',(85.2268039893037,-4.21508967804332,-1.3786452156635));
#18375=CARTESIAN_POINT('Ctrl Pts',(85.2325026476092,-4.17213209911054,-1.49826658094328));
#18376=CARTESIAN_POINT('Ctrl Pts',(85.2381971887755,-4.12920555596306,-1.61780152275365));
#18377=CARTESIAN_POINT('Ctrl Pts',(85.2438917299418,-4.08110665480784,-1.73557681927961));
#18378=CARTESIAN_POINT('Ctrl Pts',(85.2495862711081,-4.0280079617409,-1.85111881308358));
#18379=CARTESIAN_POINT('Ctrl Pts',(85.2552786797146,-3.97492915370609,-1.96661753734309));
#18380=CARTESIAN_POINT('Ctrl Pts',(85.2609710883212,-3.91685444308981,-2.07988425972799));
#18381=CARTESIAN_POINT('Ctrl Pts',(85.2666634969278,-3.85400454625176,-2.19046523767686));
#18382=CARTESIAN_POINT('Ctrl Pts',(85.2723549742321,-3.79116493192394,-2.30102812410777));
#18383=CARTESIAN_POINT('Ctrl Pts',(85.2780464515365,-3.72355188249408,-2.4089057932066));
#18384=CARTESIAN_POINT('Ctrl Pts',(85.2837379288408,-3.65143183865771,-2.5136695342938));
#18385=CARTESIAN_POINT('Ctrl Pts',(85.2894297569057,-3.57930735012866,-2.61843973187502));
#18386=CARTESIAN_POINT('Ctrl Pts',(85.2951215849706,-3.50267554109995,-2.72009529096247));
#18387=CARTESIAN_POINT('Ctrl Pts',(85.3008134130355,-3.4218456062896,-2.81823732973583));
#18388=CARTESIAN_POINT('Ctrl Pts',(85.3065068738609,-3.34099248456491,-2.91640752158208));
#18389=CARTESIAN_POINT('Ctrl Pts',(85.3122003346864,-3.25593909499697,-3.01106188008166));
#18390=CARTESIAN_POINT('Ctrl Pts',(85.3178937955118,-3.16703390178018,-3.10183578949225));
#18391=CARTESIAN_POINT('Ctrl Pts',(85.3235933098706,-3.07803418072511,-3.19270621364082));
#18392=CARTESIAN_POINT('Ctrl Pts',(85.3292928242293,-2.98517475863295,-3.27968766553765));
#18393=CARTESIAN_POINT('Ctrl Pts',(85.334992338588,-2.88884005763955,-3.36245328909966));
#18394=CARTESIAN_POINT('Ctrl Pts',(85.3406953055672,-2.79244699954045,-3.44526904996622));
#18395=CARTESIAN_POINT('Ctrl Pts',(85.3463982725464,-2.69257478182457,-3.52386364849936));
#18396=CARTESIAN_POINT('Ctrl Pts',(85.3521012395256,-2.58963866509213,-3.59795227654006));
#18397=CARTESIAN_POINT('Ctrl Pts',(85.3578123745955,-2.48655511781412,-3.67214701822872));
#18398=CARTESIAN_POINT('Ctrl Pts',(85.3635235096653,-2.38039924212008,-3.74182268439385));
#18399=CARTESIAN_POINT('Ctrl Pts',(85.3692346447352,-2.27161316217369,-3.80673910866495));
#18400=CARTESIAN_POINT('Ctrl Pts',(85.3717375787487,-2.22393710892605,-3.83518906202039));
#18401=CARTESIAN_POINT('Ctrl Pts',(85.3742405127622,-2.17575617093942,-3.86272552896489));
#18402=CARTESIAN_POINT('Ctrl Pts',(85.3767434467757,-2.1271088057357,-3.88933119296386));
#18403=CARTESIAN_POINT('Ctrl Pts',(85.3824546235107,-2.01610559955142,-3.95003980470837));
#18404=CARTESIAN_POINT('Ctrl Pts',(85.3881658002456,-1.90233012796066,-4.00608616132336));
#18405=CARTESIAN_POINT('Ctrl Pts',(85.3938769769806,-1.78621056061312,-4.05720850254878));
#18406=CARTESIAN_POINT('Ctrl Pts',(85.3995811871163,-1.67023263806625,-4.10826848379477));
#18407=CARTESIAN_POINT('Ctrl Pts',(85.405285397252,-1.55191667062105,-4.15441623982777));
#18408=CARTESIAN_POINT('Ctrl Pts',(85.4109896073877,-1.43171647466371,-4.1954352499087));
#18409=CARTESIAN_POINT('Ctrl Pts',(85.4166882782262,-1.31163300382476,-4.23641442686982));
#18410=CARTESIAN_POINT('Ctrl Pts',(85.4223869490648,-1.18966932105934,-4.27227464011371));
#18411=CARTESIAN_POINT('Ctrl Pts',(85.4280856199033,-1.06629989185179,-4.30284714353611));
#18412=CARTESIAN_POINT('Ctrl Pts',(85.4337801737631,-0.943019590326126,
-4.33339755999275));
#18413=CARTESIAN_POINT('Ctrl Pts',(85.4394747276228,-0.818335949775803,
-4.35866777406351));
#18414=CARTESIAN_POINT('Ctrl Pts',(85.4451692814826,-0.692738838989604,
-4.37853878605127));
#18415=CARTESIAN_POINT('Ctrl Pts',(85.450861702975,-0.567188758961247,-4.39840235719308));
#18416=CARTESIAN_POINT('Ctrl Pts',(85.4565541244674,-0.440726282431298,
-4.41287068393357));
#18417=CARTESIAN_POINT('Ctrl Pts',(85.4622465459597,-0.313851400797239,
-4.42187588001038));
#18418=CARTESIAN_POINT('Ctrl Pts',(85.4679380362658,-0.186997273801771,
-4.43087960298561));
#18419=CARTESIAN_POINT('Ctrl Pts',(85.4736295265719,-0.0597312739027152,
-4.4344219446511));
#18420=CARTESIAN_POINT('Ctrl Pts',(85.479321016878,0.0674420884110509,-4.43248695031477));
#18421=CARTESIAN_POINT('Ctrl Pts',(85.4850128580468,0.194623290568652,-4.43055183669204));
#18422=CARTESIAN_POINT('Ctrl Pts',(85.4907046992156,0.321711444657403,-4.42313872156896));
#18423=CARTESIAN_POINT('Ctrl Pts',(85.4963965403845,0.448203160089113,-4.41028376947404));
#18424=CARTESIAN_POINT('Ctrl Pts',(85.5020900144023,0.574731162877896,-4.39742512961004));
#18425=CARTESIAN_POINT('Ctrl Pts',(85.5077834884201,0.700661989670943,-4.37912158748894));
#18426=CARTESIAN_POINT('Ctrl Pts',(85.513476962438,0.8254989944824,-4.35546098709523));
#18427=CARTESIAN_POINT('Ctrl Pts',(85.5191764900517,0.950468732450611,-4.33177522952809));
#18428=CARTESIAN_POINT('Ctrl Pts',(85.5248760176654,1.07434193384025,-4.30272111557916));
#18429=CARTESIAN_POINT('Ctrl Pts',(85.5305755452792,1.19663344072943,-4.26843734972508));
#18430=CARTESIAN_POINT('Ctrl Pts',(85.5362785255672,1.31899902967836,-4.23413281536421));
#18431=CARTESIAN_POINT('Ctrl Pts',(85.5419815058553,1.43978063662821,-4.19459244198594));
#18432=CARTESIAN_POINT('Ctrl Pts',(85.5476844861433,1.55851099892977,-4.15000391159032));
#18433=CARTESIAN_POINT('Ctrl Pts',(85.5533956344894,1.6774114120533,-4.10535151954972));
#18434=CARTESIAN_POINT('Ctrl Pts',(85.5591067828354,1.79425434779688,-4.05563668943388));
#18435=CARTESIAN_POINT('Ctrl Pts',(85.5648179311815,1.90859480129164,-4.00109421089813));
#18436=CARTESIAN_POINT('Ctrl Pts',(85.5673207234236,1.95870213218812,-3.97719210157135));
#18437=CARTESIAN_POINT('Ctrl Pts',(85.5698235156658,2.00832921938153,-3.95236344800934));
#18438=CARTESIAN_POINT('Ctrl Pts',(85.572326307908,2.0574403354243,-3.92663065059207));
#18439=CARTESIAN_POINT('Ctrl Pts',(85.5780374789707,2.16950796136399,-3.86791047178718));
#18440=CARTESIAN_POINT('Ctrl Pts',(85.5837486500335,2.27923261035931,-3.80429821675079));
#18441=CARTESIAN_POINT('Ctrl Pts',(85.5894598210962,2.38615904545413,-3.73600508696086));
#18442=CARTESIAN_POINT('Ctrl Pts',(85.595164025495,2.4929550483602,-3.66779526325316));
#18443=CARTESIAN_POINT('Ctrl Pts',(85.6008682298937,2.59695929464167,-3.59491613750161));
#18444=CARTESIAN_POINT('Ctrl Pts',(85.6065724342925,2.69773997708178,-3.5176253376468));
#18445=CARTESIAN_POINT('Ctrl Pts',(85.6122710993368,2.79842279137251,-3.44040959490972));
#18446=CARTESIAN_POINT('Ctrl Pts',(85.617969764381,2.89588795592724,-3.35879094451206));
#18447=CARTESIAN_POINT('Ctrl Pts',(85.6236684294253,2.98973197395674,-3.27307068727529));
#18448=CARTESIAN_POINT('Ctrl Pts',(85.6293629774406,3.08350819390913,-3.18741235906428));
#18449=CARTESIAN_POINT('Ctrl Pts',(85.635057525456,3.1736681804886,-3.09765859001536));
#18450=CARTESIAN_POINT('Ctrl Pts',(85.6407520734714,3.25984129678212,-3.0041510813862));
#18451=CARTESIAN_POINT('Ctrl Pts',(85.6464444890665,3.34598214408774,-2.91067858823279));
#18452=CARTESIAN_POINT('Ctrl Pts',(85.6521369046616,3.42813881953182,-2.81345544345195));
#18453=CARTESIAN_POINT('Ctrl Pts',(85.6578293202567,3.50597761159519,-2.71286011194704));
#18454=CARTESIAN_POINT('Ctrl Pts',(85.6635208046343,3.58380367007668,-2.61228123674696));
#18455=CARTESIAN_POINT('Ctrl Pts',(85.669212289012,3.65731300600262,-2.50833158768141));
#18456=CARTESIAN_POINT('Ctrl Pts',(85.6749037733897,3.72621262094353,-2.401422183524));
#18457=CARTESIAN_POINT('Ctrl Pts',(85.6805956086053,3.79511648303695,-2.29450618919122));
#18458=CARTESIAN_POINT('Ctrl Pts',(85.686287443821,3.85940984275311,-2.18463041242818));
#18459=CARTESIAN_POINT('Ctrl Pts',(85.6919792790366,3.91884369741315,-2.07223383700904));
#18460=CARTESIAN_POINT('Ctrl Pts',(85.6976727470829,3.97829460200788,-1.95980501811048));
#18461=CARTESIAN_POINT('Ctrl Pts',(85.7033662151292,4.03288304176703,-1.84485431468707));
#18462=CARTESIAN_POINT('Ctrl Pts',(85.7090596831755,4.08240676234838,-1.72784375067082));
#18463=CARTESIAN_POINT('Ctrl Pts',(85.7147592048222,4.13198313920451,-1.61070877474976));
#18464=CARTESIAN_POINT('Ctrl Pts',(85.720458726469,4.17648388924956,-1.49150993326182));
#18465=CARTESIAN_POINT('Ctrl Pts',(85.7261582481158,4.21575545488691,-1.37072788860198));
#18466=CARTESIAN_POINT('Ctrl Pts',(85.7318612224313,4.25505081054023,-1.24987267632775));
#18467=CARTESIAN_POINT('Ctrl Pts',(85.7375641967469,4.28911056445968,-1.12743273421331));
#18468=CARTESIAN_POINT('Ctrl Pts',(85.7432671710625,4.31783184116141,-1.00390098687701));
#18469=CARTESIAN_POINT('Ctrl Pts',(85.7489783134796,4.34659425399479,-0.880192310838207));
#18470=CARTESIAN_POINT('Ctrl Pts',(85.7546894558966,4.37000284883321,-0.755389098597385));
#18471=CARTESIAN_POINT('Ctrl Pts',(85.7604005983137,4.38800629490597,-0.62999186968215));
#18472=CARTESIAN_POINT('Ctrl Pts',(85.7629034552226,4.39589614357319,-0.575037659503052));
#18473=CARTESIAN_POINT('Ctrl Pts',(85.7654063121315,4.4027485801784,-0.519969400137956));
#18474=CARTESIAN_POINT('Ctrl Pts',(85.7679091690404,4.40856243807245,-0.464829247806832));
#18475=CARTESIAN_POINT('Ctrl Pts',(85.7736203402623,4.42182885285391,-0.339007092317808));
#18476=CARTESIAN_POINT('Ctrl Pts',(85.7793315114841,4.42972492539324,-0.212422456316731));
#18477=CARTESIAN_POINT('Ctrl Pts',(85.7850426827059,4.43217402107225,-0.0855712973619365));
#18478=CARTESIAN_POINT('Ctrl Pts',(85.7907468872527,4.43462012926359,0.0411251243660879));
#18479=CARTESIAN_POINT('Ctrl Pts',(85.7964510917996,4.43163247187119,0.168087026574939));
#18480=CARTESIAN_POINT('Ctrl Pts',(85.8021552963464,4.4231860418647,0.294812209810472));
#18481=CARTESIAN_POINT('Ctrl Pts',(85.8078539615275,4.4147478142051,0.421414329939794));
#18482=CARTESIAN_POINT('Ctrl Pts',(85.8135526267087,4.4008613886107,0.547779792491482));
#18483=CARTESIAN_POINT('Ctrl Pts',(85.8192512918899,4.38155380009099,0.673405744635561));
#18484=CARTESIAN_POINT('Ctrl Pts',(85.8249458400308,4.36226016047252,0.79894093743919));
#18485=CARTESIAN_POINT('Ctrl Pts',(85.8306403881718,4.33755321349061,0.923737290004157));
#18486=CARTESIAN_POINT('Ctrl Pts',(85.8363349363128,4.30751183518414,1.04729689665758));
#18487=CARTESIAN_POINT('Ctrl Pts',(85.842027352016,4.27748170647394,1.17081023393959));
#18488=CARTESIAN_POINT('Ctrl Pts',(85.8477197677193,4.24212121245362,1.29308735892681));
#18489=CARTESIAN_POINT('Ctrl Pts',(85.8534121834226,4.2015602976528,1.41364071290682));
#18490=CARTESIAN_POINT('Ctrl Pts',(85.8591036678975,4.16100601825514,1.53417434543552));
#18491=CARTESIAN_POINT('Ctrl Pts',(85.8647951523725,4.11525313751914,1.65298438968496));
#18492=CARTESIAN_POINT('Ctrl Pts',(85.8704866368474,4.06448126504001,1.76959912017913));
#18493=CARTESIAN_POINT('Ctrl Pts',(85.8761784721493,4.01370626294856,1.88622103888362));
#18494=CARTESIAN_POINT('Ctrl Pts',(85.8818703074511,3.95791181314679,2.00064700870561));
#18495=CARTESIAN_POINT('Ctrl Pts',(85.887562142753,3.89732519136754,2.11242641356615));
#18496=CARTESIAN_POINT('Ctrl Pts',(85.8932556108743,3.83672118907633,2.22423788463581));
#18497=CARTESIAN_POINT('Ctrl Pts',(85.8989490789955,3.771322470121,2.33340092960423));
#18498=CARTESIAN_POINT('Ctrl Pts',(85.9046425471168,3.70140140394464,2.43949106308604));
#18499=CARTESIAN_POINT('Ctrl Pts',(85.9103420688211,3.63140599415773,2.54569399695831));
#18500=CARTESIAN_POINT('Ctrl Pts',(85.9160415905253,3.55687885651625,2.64881716228718));
#18501=CARTESIAN_POINT('Ctrl Pts',(85.9217411122296,3.47813487125343,2.74846626636946));
#18502=CARTESIAN_POINT('Ctrl Pts',(85.9274440865927,3.39934318442251,2.84817573593246));
#18503=CARTESIAN_POINT('Ctrl Pts',(85.9331470609559,3.31632982143383,2.94440665005461));
#18504=CARTESIAN_POINT('Ctrl Pts',(85.9388500353191,3.22944796762092,3.0368000962245));
#18505=CARTESIAN_POINT('Ctrl Pts',(85.944561177768,3.14244167726211,3.12932587291913));
#18506=CARTESIAN_POINT('Ctrl Pts',(85.9502723202169,3.05155611777546,3.21800292888566));
#18507=CARTESIAN_POINT('Ctrl Pts',(85.9559834626658,2.95717937360453,3.30251103742711));
#18508=CARTESIAN_POINT('Ctrl Pts',(85.9584863185014,2.91581963043415,3.33954594147888));
#18509=CARTESIAN_POINT('Ctrl Pts',(85.9609891743371,2.87378979081121,3.37578072053583));
#18510=CARTESIAN_POINT('Ctrl Pts',(85.9634920301727,2.83112429126425,3.41119103062457));
#18511=CARTESIAN_POINT('Ctrl Pts',(85.9692032026784,2.73376749408617,3.49199248411575));
#18512=CARTESIAN_POINT('Ctrl Pts',(85.9749143751842,2.63279861011643,3.56874735740786));
#18513=CARTESIAN_POINT('Ctrl Pts',(85.9806255476899,2.52858789811429,3.64111689478791));
#18514=CARTESIAN_POINT('Ctrl Pts',(85.9863297535422,2.42450430535391,3.7133981537123));
#18515=CARTESIAN_POINT('Ctrl Pts',(85.9920339593944,2.31718707696461,3.78130449344741));
#18516=CARTESIAN_POINT('Ctrl Pts',(85.9977381652467,2.20704029072567,3.84453666325522));
#18517=CARTESIAN_POINT('Ctrl Pts',(86.0034368317531,2.09700046786776,3.90770742839655));
#18518=CARTESIAN_POINT('Ctrl Pts',(86.0091354982595,1.98413689906786,3.96621285812227));
#18519=CARTESIAN_POINT('Ctrl Pts',(86.0148341647659,1.8688830600145,4.01979665007956));
#18520=CARTESIAN_POINT('Ctrl Pts',(86.0205287142502,1.75371248651015,4.07334173023434));
#18521=CARTESIAN_POINT('Ctrl Pts',(86.0262232637346,1.63615544044178,4.1219720817462));
#18522=CARTESIAN_POINT('Ctrl Pts',(86.031917813219,1.51667002306284,4.165477288516));
#18523=CARTESIAN_POINT('Ctrl Pts',(86.0376102302877,1.39722934891961,4.20896620406161));
#18524=CARTESIAN_POINT('Ctrl Pts',(86.0433026473565,1.27586211372183,4.24733365451933));
#18525=CARTESIAN_POINT('Ctrl Pts',(86.0489950644252,1.15304612211939,4.28041746098035));
#18526=CARTESIAN_POINT('Ctrl Pts',(86.054686550279,1.03025022182269,4.31349585530519));
#18527=CARTESIAN_POINT('Ctrl Pts',(86.0603780361328,0.906006421814709,4.34129222110404));
#18528=CARTESIAN_POINT('Ctrl Pts',(86.0660695219865,0.780806886217592,4.36369449050173));
#18529=CARTESIAN_POINT('Ctrl Pts',(86.0717613586791,0.655599632977198,4.38609814083685));
#18530=CARTESIAN_POINT('Ctrl Pts',(86.0774531953717,0.529436919905267,4.40310696314175));
#18531=CARTESIAN_POINT('Ctrl Pts',(86.0831450320643,0.402819771366682,4.41466026233006));
#18532=CARTESIAN_POINT('Ctrl Pts',(86.0888385015867,0.276166299885106,4.42621687583899));
#18533=CARTESIAN_POINT('Ctrl Pts',(86.0945319711091,0.14905853094495,4.43231481657198));
#18534=CARTESIAN_POINT('Ctrl Pts',(86.1002254406316,0.0220007440576986,
4.43294540540044));
#18535=CARTESIAN_POINT('Ctrl Pts',(86.1059249637453,-0.105192137239539,
4.43357666470356));
#18536=CARTESIAN_POINT('Ctrl Pts',(86.111624486859,-0.232334530872,4.42872896347229));
#18537=CARTESIAN_POINT('Ctrl Pts',(86.1173240099726,-0.358923714736252,
4.41844574109493));
#18538=CARTESIAN_POINT('Ctrl Pts',(86.1230269857519,-0.485589583983631,
4.4081562893319));
#18539=CARTESIAN_POINT('Ctrl Pts',(86.1287299615311,-0.611701180417469,
4.39242480622584));
#18540=CARTESIAN_POINT('Ctrl Pts',(86.1344329373103,-0.736763988310469,
4.37134622576717));
#18541=CARTESIAN_POINT('Ctrl Pts',(86.1401440811732,-0.862005917335847,
4.35023745552414));
#18542=CARTESIAN_POINT('Ctrl Pts',(86.1458552250361,-0.986195668909993,
4.32376637898218));
#18543=CARTESIAN_POINT('Ctrl Pts',(86.151566368899,-1.10885157311499,4.29207842295553));
#18544=CARTESIAN_POINT('Ctrl Pts',(86.154069209701,-1.16260406281344,4.27819155349802));
#18545=CARTESIAN_POINT('Ctrl Pts',(86.1565720505031,-1.21606220092094,4.26330340480065));
#18546=CARTESIAN_POINT('Ctrl Pts',(86.1590748913052,-1.26918663554271,4.24742913821523));
#18547=CARTESIAN_POINT('Ctrl Pts',(86.1647860630679,-1.39040999528434,4.21120603405196));
#18548=CARTESIAN_POINT('Ctrl Pts',(86.1704972348306,-1.51026837993683,4.16973328146862));
#18549=CARTESIAN_POINT('Ctrl Pts',(86.1762084065934,-1.62827458282358,4.12313119885006));
#18550=CARTESIAN_POINT('Ctrl Pts',(86.1819126116936,-1.74613683812524,4.07658596288097));
#18551=CARTESIAN_POINT('Ctrl Pts',(86.1876168167939,-1.86215103851585,4.02492399025031));
#18552=CARTESIAN_POINT('Ctrl Pts',(86.1933210218942,-1.97584410367757,3.96831564747093));
#18553=CARTESIAN_POINT('Ctrl Pts',(86.1990196876406,-2.08942676149783,3.91176227705615));
#18554=CARTESIAN_POINT('Ctrl Pts',(86.204718353387,-2.20069241403268,3.85027227151843));
#18555=CARTESIAN_POINT('Ctrl Pts',(86.2104170191334,-2.30918742425279,3.78406427530939));
#18556=CARTESIAN_POINT('Ctrl Pts',(86.2161115678507,-2.41760405171904,3.71790411139291));
#18557=CARTESIAN_POINT('Ctrl Pts',(86.221806116568,-2.52325368122513,3.64703294803797));
#18558=CARTESIAN_POINT('Ctrl Pts',(86.2275006652853,-2.62570720997412,3.57171536484781));
#18559=CARTESIAN_POINT('Ctrl Pts',(86.2331930815794,-2.72812237320855,3.4964259856431));
#18560=CARTESIAN_POINT('Ctrl Pts',(86.2388854978734,-2.82734349431179,3.41669373329982));
#18561=CARTESIAN_POINT('Ctrl Pts',(86.2445779141674,-2.92297069027303,3.33282632967948));
#18562=CARTESIAN_POINT('Ctrl Pts',(86.2502693992418,-3.01858224262913,3.24897264588575));
#18563=CARTESIAN_POINT('Ctrl Pts',(86.2559608843163,-3.11060073929695,3.16098541946339));
#18564=CARTESIAN_POINT('Ctrl Pts',(86.2616523693908,-3.19866003939449,3.06921210612444));
#18565=CARTESIAN_POINT('Ctrl Pts',(86.2673442053004,-3.28672476765249,2.97743313568545));
#18566=CARTESIAN_POINT('Ctrl Pts',(86.27303604121,-3.3708295375752,2.88186790218265));
#18567=CARTESIAN_POINT('Ctrl Pts',(86.2787278771196,-3.45064604946544,2.78289971815525));
#18568=CARTESIAN_POINT('Ctrl Pts',(86.2844213458561,-3.53048545845897,2.68390314295066));
#18569=CARTESIAN_POINT('Ctrl Pts',(86.2901148145927,-3.60603391168587,2.58150198578219));
#18570=CARTESIAN_POINT('Ctrl Pts',(86.2958082833293,-3.6770045935842,2.47611110791917));
#18571=CARTESIAN_POINT('Ctrl Pts',(86.301507805657,-3.74805073519088,2.37060817301099));
#18572=CARTESIAN_POINT('Ctrl Pts',(86.3072073279847,-3.81450916416067,2.26210950190459));
#18573=CARTESIAN_POINT('Ctrl Pts',(86.3129068503124,-3.87613730269169,2.15105755633874));
#18574=CARTESIAN_POINT('Ctrl Pts',(86.3186098253045,-3.93780277440074,2.03993833757344));
#18575=CARTESIAN_POINT('Ctrl Pts',(86.3243128002966,-3.99463194833798,1.92626311952929));
#18576=CARTESIAN_POINT('Ctrl Pts',(86.3300157752888,-4.04642965167852,1.8104960850598));
#18577=CARTESIAN_POINT('Ctrl Pts',(86.3357269183697,-4.09830154230549,1.69456324319747));
#18578=CARTESIAN_POINT('Ctrl Pts',(86.3414380614506,-4.14512742613423,1.57653297279318));
#18579=CARTESIAN_POINT('Ctrl Pts',(86.3471492045315,-4.18676127389963,1.45688676134225));
#18580=CARTESIAN_POINT('Ctrl Pts',(86.3496520538335,-4.20500687645996,1.40445304841033));
#18581=CARTESIAN_POINT('Ctrl Pts',(86.3521549031355,-4.22225598356386,1.35170915067926));
#18582=CARTESIAN_POINT('Ctrl Pts',(86.3546577524375,-4.23849939450282,1.29869622421843));
#18583=CARTESIAN_POINT('Ctrl Pts',(86.361543519039,-4.28318779681662,1.1528485944062));
#18584=CARTESIAN_POINT('Ctrl Pts',(86.3684292856406,-4.32037172905848,1.00460305815416));
#18585=CARTESIAN_POINT('Ctrl Pts',(86.3753150522421,-4.34983235093349,0.854662224959333));
#18586=CARTESIAN_POINT('Ctrl Pts',(86.3821258148638,-4.37897206970221,0.706354638996579));
#18587=CARTESIAN_POINT('Ctrl Pts',(86.3889365774854,-4.40055579046778,0.556388511698405));
#18588=CARTESIAN_POINT('Ctrl Pts',(86.3957473401071,-4.41441820880992,0.405463781030341));
#18589=CARTESIAN_POINT('Ctrl Pts',(86.4017675963939,-4.42667165468834,0.272056465415288));
#18590=CARTESIAN_POINT('Ctrl Pts',(86.4077878526808,-4.43289274202569,0.137900439209401));
#18591=CARTESIAN_POINT('Ctrl Pts',(86.4138081089676,-4.43299862449031,0.00349217224992315));
#18592=CARTESIAN_POINT('',(87.6638081644291,-4.43227616981233,-0.00345667368086795));
#18593=CARTESIAN_POINT('Ctrl Pts',(86.4138081402417,-4.43034383484303,0.0034893830850436));
#18594=CARTESIAN_POINT('Ctrl Pts',(86.4592856313511,-4.42253105442582,-1.01124001134147));
#18595=CARTESIAN_POINT('Ctrl Pts',(86.5699574095046,-3.57721990853862,-3.49240746487907));
#18596=CARTESIAN_POINT('Ctrl Pts',(86.7458234747023,0.510683341348773,-5.18931099460031));
#18597=CARTESIAN_POINT('Ctrl Pts',(86.9414063358345,4.60181158071817,-2.45215751524593));
#18598=CARTESIAN_POINT('Ctrl Pts',(87.1369891969671,4.59217127324197,2.47016372199963));
#18599=CARTESIAN_POINT('Ctrl Pts',(87.3325720580992,0.490353289406007,5.19127149832776));
#18600=CARTESIAN_POINT('Ctrl Pts',(87.5081783725243,-3.58484425455734,3.48089885108923));
#18601=CARTESIAN_POINT('Ctrl Pts',(87.618590399905,-4.42252617546647,1.00556395309676));
#18602=CARTESIAN_POINT('Ctrl Pts',(87.6638081402417,-4.43019710367684,-0.00345451242541441));
#18603=CARTESIAN_POINT('',(88.9138081402808,-4.43299954096812,0.00201736869289629));
#18604=CARTESIAN_POINT('Ctrl Pts',(87.6638081728344,-4.4329986517271,-0.00345742472382504));
#18605=CARTESIAN_POINT('Ctrl Pts',(87.6705757511896,-4.43288079608067,-0.154568139619312));
#18606=CARTESIAN_POINT('Ctrl Pts',(87.6773433295449,-4.42503256386582,-0.305361128860425));
#18607=CARTESIAN_POINT('Ctrl Pts',(87.6841109079001,-4.40957434100509,-0.455129795936879));
#18608=CARTESIAN_POINT('Ctrl Pts',(87.6909538833469,-4.39394389922306,-0.606567024692115));
#18609=CARTESIAN_POINT('Ctrl Pts',(87.6977968587938,-4.37053302507896,-0.756956934271215));
#18610=CARTESIAN_POINT('Ctrl Pts',(87.7046398342406,-4.33951570976822,-0.905589534322728));
#18611=CARTESIAN_POINT('Ctrl Pts',(87.7110058162818,-4.31066047365515,-1.04386161640392));
#18612=CARTESIAN_POINT('Ctrl Pts',(87.7173717983229,-4.27522281140193,-1.1806130378423));
#18613=CARTESIAN_POINT('Ctrl Pts',(87.7237377803641,-4.23337995783103,-1.31528823177072));
#18614=CARTESIAN_POINT('Ctrl Pts',(87.7294489573705,-4.19584106098065,-1.43611073266965));
#18615=CARTESIAN_POINT('Ctrl Pts',(87.7351601343769,-4.1530676566428,-1.55551126187134));
#18616=CARTESIAN_POINT('Ctrl Pts',(87.7408713113832,-4.1051853535367,-1.67300394892175));
#18617=CARTESIAN_POINT('Ctrl Pts',(87.7465755217392,-4.05736145857781,-1.79035331516853));
#18618=CARTESIAN_POINT('Ctrl Pts',(87.7522797320952,-4.00444121260155,-1.90579910278776));
#18619=CARTESIAN_POINT('Ctrl Pts',(87.7579839424511,-3.94660011590412,-2.01887011101397));
#18620=CARTESIAN_POINT('Ctrl Pts',(87.7636826134589,-3.88881518858871,-2.13183131619322));
#18621=CARTESIAN_POINT('Ctrl Pts',(87.7693812844667,-3.82611910009916,-2.24242197751844));
#18622=CARTESIAN_POINT('Ctrl Pts',(87.7750799554746,-3.75873541441771,-2.35019086127109));
#18623=CARTESIAN_POINT('Ctrl Pts',(87.7807745094528,-3.69140041037253,-2.45788188692578));
#18624=CARTESIAN_POINT('Ctrl Pts',(87.786469063431,-3.6193847603393,-2.56275485516058));
#18625=CARTESIAN_POINT('Ctrl Pts',(87.7921636174092,-3.54295769399091,-2.66438356446489));
#18626=CARTESIAN_POINT('Ctrl Pts',(87.7978560389441,-3.46655924733509,-2.76597421680122));
#18627=CARTESIAN_POINT('Ctrl Pts',(87.8035484604791,-3.3857529085027,-2.86432270729645));
#18628=CARTESIAN_POINT('Ctrl Pts',(87.809240882014,-3.30085072918975,-2.95903252155287));
#18629=CARTESIAN_POINT('Ctrl Pts',(87.8149323723154,-3.21596243917818,-3.05372684205912));
#18630=CARTESIAN_POINT('Ctrl Pts',(87.8206238626167,-3.12697990780726,-3.14478337323757));
#18631=CARTESIAN_POINT('Ctrl Pts',(87.8263153529181,-3.03425455143084,-3.23183977281072));
#18632=CARTESIAN_POINT('Ctrl Pts',(87.832007194035,-2.94152347959329,-3.31890153841843));
#18633=CARTESIAN_POINT('Ctrl Pts',(87.8376990351518,-2.84504941492009,-3.40196240881344));
#18634=CARTESIAN_POINT('Ctrl Pts',(87.8433908762687,-2.74521921707215,-3.48069827049369));
#18635=CARTESIAN_POINT('Ctrl Pts',(87.8490843501873,-2.64536038122838,-3.55945671889947));
#18636=CARTESIAN_POINT('Ctrl Pts',(87.8547778241059,-2.5421438102242,-3.63388744331551));
#18637=CARTESIAN_POINT('Ctrl Pts',(87.8604712980245,-2.43598745958902,-3.70370815490706));
#18638=CARTESIAN_POINT('Ctrl Pts',(87.8661708254683,-2.32971823935071,-3.77360310262259));
#18639=CARTESIAN_POINT('Ctrl Pts',(87.8718703529121,-2.22050333247716,-3.83887803149167));
#18640=CARTESIAN_POINT('Ctrl Pts',(87.8775698803559,-2.10878781240466,-3.89929518788377));
#18641=CARTESIAN_POINT('Ctrl Pts',(87.8832728604334,-1.99700461781569,-3.95974894350437));
#18642=CARTESIAN_POINT('Ctrl Pts',(87.8889758405108,-1.8827181507044,-4.01533889009331));
#18643=CARTESIAN_POINT('Ctrl Pts',(87.8946788205883,-1.76639468899386,-4.06587491232752));
#18644=CARTESIAN_POINT('Ctrl Pts',(87.9003899686633,-1.64990462495538,-4.11648331393236));
#18645=CARTESIAN_POINT('Ctrl Pts',(87.9061011167384,-1.53137211262844,-4.16202319497411));
#18646=CARTESIAN_POINT('Ctrl Pts',(87.9118122648134,-1.41128019930832,-4.20235376890621));
#18647=CARTESIAN_POINT('Ctrl Pts',(87.9143150570411,-1.35865240830802,-4.22002780670894));
#18648=CARTESIAN_POINT('Ctrl Pts',(87.9168178492688,-1.30572529828921,-4.2367020811707));
#18649=CARTESIAN_POINT('Ctrl Pts',(87.9193206414965,-1.25254012004275,-4.25236784011958));
#18650=CARTESIAN_POINT('Ctrl Pts',(87.9250318052834,-1.13117596498531,-4.28811579962354));
#18651=CARTESIAN_POINT('Ctrl Pts',(87.9307429690702,-1.00809299213488,-4.31871910368859));
#18652=CARTESIAN_POINT('Ctrl Pts',(87.936454132857,-0.883765194782438,-4.34401290058986));
#18653=CARTESIAN_POINT('Ctrl Pts',(87.94215833,-0.759589056096376,-4.36927584338138));
#18654=CARTESIAN_POINT('Ctrl Pts',(87.947862527143,-0.634171501678992,-4.38924208537194));
#18655=CARTESIAN_POINT('Ctrl Pts',(87.953566724286,-0.508001978349318,-4.403796429218));
#18656=CARTESIAN_POINT('Ctrl Pts',(87.9592653821028,-0.381954977810399,
-4.41833663939073));
#18657=CARTESIAN_POINT('Ctrl Pts',(87.9649640399195,-0.255157855715425,
-4.42747536357883));
#18658=CARTESIAN_POINT('Ctrl Pts',(87.9706626977363,-0.128110090345371,
-4.43114847469047));
#18659=CARTESIAN_POINT('Ctrl Pts',(87.9763572385605,-0.00115411057021916,
-4.43481893216482));
#18660=CARTESIAN_POINT('Ctrl Pts',(87.9820517793847,0.12605175445124,-4.43303162403448));
#18661=CARTESIAN_POINT('Ctrl Pts',(87.987746320209,0.253003539893165,-4.42577430613012));
#18662=CARTESIAN_POINT('Ctrl Pts',(87.9934387286927,0.379907787798938,-4.4185197057536));
#18663=CARTESIAN_POINT('Ctrl Pts',(87.9991311371764,0.506557747435535,-4.40579919098026));
#18664=CARTESIAN_POINT('Ctrl Pts',(88.00482354566,0.63245041801114,-4.38765261486795));
#18665=CARTESIAN_POINT('Ctrl Pts',(88.010515022978,0.758322495028929,-4.36950900717757));
#18666=CARTESIAN_POINT('Ctrl Pts',(88.0162065002959,0.883437134455935,-4.34594116058187));
#18667=CARTESIAN_POINT('Ctrl Pts',(88.0218979776139,1.00729794900592,-4.31704063473214));
#18668=CARTESIAN_POINT('Ctrl Pts',(88.0275898058288,1.13116639995466,-4.28813832707643));
#18669=CARTESIAN_POINT('Ctrl Pts',(88.0332816340438,1.2537804835487,-4.25390277696927));
#18670=CARTESIAN_POINT('Ctrl Pts',(88.0389734622587,1.37465597623267,-4.21447623637953));
#18671=CARTESIAN_POINT('Ctrl Pts',(88.0446669233707,1.49556614621698,-4.17503838492803));
#18672=CARTESIAN_POINT('Ctrl Pts',(88.0503603844827,1.61473635372315,-4.13040670415919));
#18673=CARTESIAN_POINT('Ctrl Pts',(88.0560538455948,1.73169994193205,-4.0807725140116));
#18674=CARTESIAN_POINT('Ctrl Pts',(88.0617533604442,1.84878789506444,-4.03108554887347));
#18675=CARTESIAN_POINT('Ctrl Pts',(88.0674528752937,1.96366417657744,-3.97638561031657));
#18676=CARTESIAN_POINT('Ctrl Pts',(88.0731523901432,2.07588415770217,-3.91691127852051));
#18677=CARTESIAN_POINT('Ctrl Pts',(88.0788553577306,2.18817212113683,-3.85740091746819));
#18678=CARTESIAN_POINT('Ctrl Pts',(88.084558325318,2.29780023476497,-3.7931106029559));
#18679=CARTESIAN_POINT('Ctrl Pts',(88.0902612929054,2.4043517590273,-3.72432297456361));
#18680=CARTESIAN_POINT('Ctrl Pts',(88.0959724287579,2.51105589525509,-3.65543682280207));
#18681=CARTESIAN_POINT('Ctrl Pts',(88.1016835646103,2.61467431828384,-3.58204072535583));
#18682=CARTESIAN_POINT('Ctrl Pts',(88.1073947004628,2.71482204360294,-3.50445862745839));
#18683=CARTESIAN_POINT('Ctrl Pts',(88.1098976345181,2.75871228868591,-3.47045788226004));
#18684=CARTESIAN_POINT('Ctrl Pts',(88.1124005685735,2.80193638633805,-3.43565363688784));
#18685=CARTESIAN_POINT('Ctrl Pts',(88.1149035026288,2.84446417661572,-3.40007537386304));
#18686=CARTESIAN_POINT('Ctrl Pts',(88.1206146717402,2.94150364982505,-3.31889326025948));
#18687=CARTESIAN_POINT('Ctrl Pts',(88.1263258408516,3.03521459496464,-3.23342829836434));
#18688=CARTESIAN_POINT('Ctrl Pts',(88.1320370099629,3.12519701718668,-3.1439835565358));
#18689=CARTESIAN_POINT('Ctrl Pts',(88.1377412123272,3.21506967470595,-3.05464792352271));
#18690=CARTESIAN_POINT('Ctrl Pts',(88.1434454146914,3.3012225772479,-2.96134244794028));
#18691=CARTESIAN_POINT('Ctrl Pts',(88.1491496170557,3.38328848545012,-2.86441058932211));
#18692=CARTESIAN_POINT('Ctrl Pts',(88.1548482799858,3.46527469825097,-2.76757286264675));
#18693=CARTESIAN_POINT('Ctrl Pts',(88.1605469429159,3.5431815578693,-2.66711606340454));
#18694=CARTESIAN_POINT('Ctrl Pts',(88.1662456058459,3.61667876495443,-2.56342031495573));
#18695=CARTESIAN_POINT('Ctrl Pts',(88.1719401516709,3.6901228726136,-2.45979948343144));
#18696=CARTESIAN_POINT('Ctrl Pts',(88.1776346974958,3.75916343848788,-2.3529446846301));
#18697=CARTESIAN_POINT('Ctrl Pts',(88.1833292433207,3.82351085388271,-2.24326854171344));
#18698=CARTESIAN_POINT('Ctrl Pts',(88.189021656621,3.88783417210612,-2.13363347091754));
#18699=CARTESIAN_POINT('Ctrl Pts',(88.1947140699213,3.94746763271936,-2.02117950050547));
#18700=CARTESIAN_POINT('Ctrl Pts',(88.2004064832217,4.0021655180592,-1.90634733615308));
#18701=CARTESIAN_POINT('Ctrl Pts',(88.2060979652404,4.05685445479885,-1.79153395839767));
#18702=CARTESIAN_POINT('Ctrl Pts',(88.2117894472592,4.10660925078805,-1.67434352083793));
#18703=CARTESIAN_POINT('Ctrl Pts',(88.217480929278,4.15123088658256,-1.55523989348363));
#18704=CARTESIAN_POINT('Ctrl Pts',(88.2231727620735,4.19585527249231,-1.43612892554904));
#18705=CARTESIAN_POINT('Ctrl Pts',(88.228864594869,4.23534572894581,-1.31510490710335));
#18706=CARTESIAN_POINT('Ctrl Pts',(88.2345564276645,4.26955216788328,-1.19264969111771));
#18707=CARTESIAN_POINT('Ctrl Pts',(88.2402498932322,4.30376841935809,-1.07015934734863));
#18708=CARTESIAN_POINT('Ctrl Pts',(88.2459433587999,4.33269753054817,-0.946237373589296));
#18709=CARTESIAN_POINT('Ctrl Pts',(88.2516368243676,4.35623998860488,-0.821378208671102));
#18710=CARTESIAN_POINT('Ctrl Pts',(88.2573363434618,4.37980747797038,-0.696386288358162));
#18711=CARTESIAN_POINT('Ctrl Pts',(88.263035862556,4.397976804961,-0.570455579934879));
#18712=CARTESIAN_POINT('Ctrl Pts',(88.2687353816502,4.41070000104378,-0.444088392994422));
#18713=CARTESIAN_POINT('Ctrl Pts',(88.2744383533676,4.42343090451393,-0.317644656038224));
#18714=CARTESIAN_POINT('Ctrl Pts',(88.280141325085,4.43070908200215,-0.19076431168318));
#18715=CARTESIAN_POINT('Ctrl Pts',(88.2858442968024,4.43253869514335,-0.0639508878508889));
#18716=CARTESIAN_POINT('Ctrl Pts',(88.2915554365745,4.43437092873946,0.0630441639184597));
#18717=CARTESIAN_POINT('Ctrl Pts',(88.2972665763467,4.43073902727015,0.189971705676443));
#18718=CARTESIAN_POINT('Ctrl Pts',(88.3029777161188,4.42169913418975,0.316331735217335));
#18719=CARTESIAN_POINT('Ctrl Pts',(88.3054805986663,4.41773743976013,0.371708477033451));
#18720=CARTESIAN_POINT('Ctrl Pts',(88.3079834812138,4.41273775705088,0.426976332165075));
#18721=CARTESIAN_POINT('Ctrl Pts',(88.3104863637613,4.40670789966582,0.482093857068187));
#18722=CARTESIAN_POINT('Ctrl Pts',(88.3161975759169,4.39294864642833,0.60786399299958));
#18723=CARTESIAN_POINT('Ctrl Pts',(88.3219087880726,4.37377955462869,0.733238601419334));
#18724=CARTESIAN_POINT('Ctrl Pts',(88.3276200002283,4.34923107730234,0.857716757576488));
#18725=CARTESIAN_POINT('Ctrl Pts',(88.3333242458431,4.3247125442268,0.982043075186615));
#18726=CARTESIAN_POINT('Ctrl Pts',(88.339028491458,4.2948277567347,1.10547472776412));
#18727=CARTESIAN_POINT('Ctrl Pts',(88.3447327370728,4.25965894325909,1.22751565656527));
#18728=CARTESIAN_POINT('Ctrl Pts',(88.3504314434066,4.2245242815287,1.34943807381331));
#18729=CARTESIAN_POINT('Ctrl Pts',(88.3561301497404,4.18411591410322,1.46997207321479));
#18730=CARTESIAN_POINT('Ctrl Pts',(88.3618288560741,4.13856706284499,1.58863201098763));
#18731=CARTESIAN_POINT('Ctrl Pts',(88.3675234454031,4.09305111815007,1.70720622342061));
#18732=CARTESIAN_POINT('Ctrl Pts',(88.373218034732,4.04240222360458,1.82390869754284));
#18733=CARTESIAN_POINT('Ctrl Pts',(88.378912624061,3.98680320857934,1.93826963450947));
#18734=CARTESIAN_POINT('Ctrl Pts',(88.3846050808537,3.9312250145309,2.05258774506246));
#18735=CARTESIAN_POINT('Ctrl Pts',(88.3902975376465,3.87070056010836,2.16456570357824));
#18736=CARTESIAN_POINT('Ctrl Pts',(88.3959899944392,3.80546038042305,2.27375466861103));
#18737=CARTESIAN_POINT('Ctrl Pts',(88.4016815199299,3.74023087421623,2.38292577001936));
#18738=CARTESIAN_POINT('Ctrl Pts',(88.4073730454205,3.67028738199691,2.48930844301699));
#18739=CARTESIAN_POINT('Ctrl Pts',(88.4130645709112,3.59590560802497,2.59247986649357));
#18740=CARTESIAN_POINT('Ctrl Pts',(88.4187564471111,3.52151925068205,2.69565764734622));
#18741=CARTESIAN_POINT('Ctrl Pts',(88.4244483233109,3.44269430109197,2.79562346133372));
#18742=CARTESIAN_POINT('Ctrl Pts',(88.4301401995108,3.35974855879223,2.89198523884433));
#18743=CARTESIAN_POINT('Ctrl Pts',(88.4358337083682,3.27677902433815,2.98837465676445));
#18744=CARTESIAN_POINT('Ctrl Pts',(88.4415272172257,3.18968660604424,3.08115767926207));
#18745=CARTESIAN_POINT('Ctrl Pts',(88.4472207260832,3.09882761858552,3.1699773485455));
#18746=CARTESIAN_POINT('Ctrl Pts',(88.4529202880598,3.00787203335399,3.25889144747728));
#18747=CARTESIAN_POINT('Ctrl Pts',(88.4586198500364,2.91314216926165,3.34383350083435));
#18748=CARTESIAN_POINT('Ctrl Pts',(88.464319412013,2.8150294694347,3.42448508336862));
#18749=CARTESIAN_POINT('Ctrl Pts',(88.4700224264379,2.71685733889655,3.50518551973035));
#18750=CARTESIAN_POINT('Ctrl Pts',(88.4757254408628,2.61529860898164,3.58159006836629));
#18751=CARTESIAN_POINT('Ctrl Pts',(88.4814284552876,2.51077463990583,3.65342301240984));
#18752=CARTESIAN_POINT('Ctrl Pts',(88.4871396371286,2.40610097968761,3.72535883003875));
#18753=CARTESIAN_POINT('Ctrl Pts',(88.4928508189695,2.29845393850136,3.79270975882326));
#18754=CARTESIAN_POINT('Ctrl Pts',(88.4985620008105,2.18828076329471,3.85524529712369));
#18755=CARTESIAN_POINT('Ctrl Pts',(88.5010644088382,2.14000735058376,3.882645831272));
#18756=CARTESIAN_POINT('Ctrl Pts',(88.5035668168659,2.0912492400767,3.90912250451395));
#18757=CARTESIAN_POINT('Ctrl Pts',(88.5060692248936,2.04204523170036,3.93465885073787));
#18758=CARTESIAN_POINT('Ctrl Pts',(88.5117803174121,1.92974993812405,3.99293888910686));
#18759=CARTESIAN_POINT('Ctrl Pts',(88.5174914099306,1.81478444621793,4.04649764867552));
#18760=CARTESIAN_POINT('Ctrl Pts',(88.5232025024492,1.69758250154027,4.09508274036854));
#18761=CARTESIAN_POINT('Ctrl Pts',(88.5289066283904,1.58052352362568,4.14360856637862));
#18762=CARTESIAN_POINT('Ctrl Pts',(88.5346107543316,1.46123388602126,4.18717264322623));
#18763=CARTESIAN_POINT('Ctrl Pts',(88.5403148802727,1.34017199207094,4.2255683678848));
#18764=CARTESIAN_POINT('Ctrl Pts',(88.5460134670361,1.21922765922719,4.26392680712076));
#18765=CARTESIAN_POINT('Ctrl Pts',(88.5517120537995,1.09651487294086,4.29712676105349));
#18766=CARTESIAN_POINT('Ctrl Pts',(88.5574106405628,0.972511642647691,4.32500983870727));
#18767=CARTESIAN_POINT('Ctrl Pts',(88.5631051105638,0.848597994537073,4.35287277312005));
#18768=CARTESIAN_POINT('Ctrl Pts',(88.5687995805647,0.723396145975541,4.37542638874733));
#18769=CARTESIAN_POINT('Ctrl Pts',(88.5744940505657,0.597398424925402,4.39256236403044));
#18770=CARTESIAN_POINT('Ctrl Pts',(88.5801863888238,0.471447871519799,4.40969192440712));
#18771=CARTESIAN_POINT('Ctrl Pts',(88.5858787270819,0.344702432910642,4.4214078232891));
#18772=CARTESIAN_POINT('Ctrl Pts',(88.59157106534,0.217663446340325,4.42765306049686));
#18773=CARTESIAN_POINT('Ctrl Pts',(88.5972624728252,0.0906452323342379,
4.43389727652527));
#18774=CARTESIAN_POINT('Ctrl Pts',(88.6029538803103,-0.0366660356143475,
4.43467259057519));
#18775=CARTESIAN_POINT('Ctrl Pts',(88.6086452877954,-0.163765631212743,
4.42997402001789));
#18776=CARTESIAN_POINT('Ctrl Pts',(88.6143370466438,-0.29087307340105,4.42527515939078));
#18777=CARTESIAN_POINT('Ctrl Pts',(88.6200288054923,-0.41776841833657,4.41510175678727));
#18778=CARTESIAN_POINT('Ctrl Pts',(88.6257205643407,-0.543949192591837,
4.39950091213523));
#18779=CARTESIAN_POINT('Ctrl Pts',(88.6314139566265,-0.670166178569389,
4.38389559030781));
#18780=CARTESIAN_POINT('Ctrl Pts',(88.6371073489123,-0.795667789915656,
4.36285977682147));
#18781=CARTESIAN_POINT('Ctrl Pts',(88.6428007411982,-0.919959420052621,
4.3364920921704));
#18782=CARTESIAN_POINT('Ctrl Pts',(88.6485001884044,-1.04438323428812,4.31009636549734));
#18783=CARTESIAN_POINT('Ctrl Pts',(88.6541996356106,-1.1675941072211,4.27835752889874));
#18784=CARTESIAN_POINT('Ctrl Pts',(88.6598990828168,-1.2891100236671,4.24142480151199));
#18785=CARTESIAN_POINT('Ctrl Pts',(88.6656019833454,-1.41069956718979,4.20446969640855));
#18786=CARTESIAN_POINT('Ctrl Pts',(88.671304883874,-1.5305917324047,4.16231456350746));
#18787=CARTESIAN_POINT('Ctrl Pts',(88.6770077844026,-1.64832346061325,4.11515719860031));
#18788=CARTESIAN_POINT('Ctrl Pts',(88.6827188546696,-1.76622384640437,4.06793227801138));
#18789=CARTESIAN_POINT('Ctrl Pts',(88.6884299249366,-1.88195725229094,4.01569098048937));
#18790=CARTESIAN_POINT('Ctrl Pts',(88.6941409952036,-1.99508389680263,3.95867771417665));
#18791=CARTESIAN_POINT('Ctrl Pts',(88.6966446921444,-2.04467789942275,3.93368346024911));
#18792=CARTESIAN_POINT('Ctrl Pts',(88.6991483890852,-2.0937712691401,3.90777266002725));
#18793=CARTESIAN_POINT('Ctrl Pts',(88.7016520860259,-2.14232873571998,3.88096851161001));
#18794=CARTESIAN_POINT('Ctrl Pts',(88.707363269979,-2.2530931894419,3.81982555943327));
#18795=CARTESIAN_POINT('Ctrl Pts',(88.713074453932,-2.36140886395185,3.75384261937051));
#18796=CARTESIAN_POINT('Ctrl Pts',(88.718785637885,-2.46682521991997,3.68324073804127));
#18797=CARTESIAN_POINT('Ctrl Pts',(88.7244898544835,-2.572112973285,3.61272498742333));
#18798=CARTESIAN_POINT('Ctrl Pts',(88.730194071082,-2.67450811614117,3.53760172623251));
#18799=CARTESIAN_POINT('Ctrl Pts',(88.7358982876806,-2.77358454238318,3.4581379073503));
#18800=CARTESIAN_POINT('Ctrl Pts',(88.7415969642293,-2.87256474360949,3.37875126532548));
#18801=CARTESIAN_POINT('Ctrl Pts',(88.7472956407781,-2.96823233231395,3.29503270245464));
#18802=CARTESIAN_POINT('Ctrl Pts',(88.7529943173268,-3.06019045529571,3.2072922188845));
#18803=CARTESIAN_POINT('Ctrl Pts',(88.7586888761462,-3.15208213150448,3.11961513452048));
#18804=CARTESIAN_POINT('Ctrl Pts',(88.7643834349655,-3.24026938893768,3.02792218817119));
#18805=CARTESIAN_POINT('Ctrl Pts',(88.7700779937849,-3.32438910454279,2.93256305671288));
#18806=CARTESIAN_POINT('Ctrl Pts',(88.7757704191134,-3.40847730433697,2.83723965196068));
#18807=CARTESIAN_POINT('Ctrl Pts',(88.781462844442,-3.4885007287481,2.73825309203292));
#18808=CARTESIAN_POINT('Ctrl Pts',(88.7871552697705,-3.56413397044426,2.63598900618444));
#18809=CARTESIAN_POINT('Ctrl Pts',(88.7928467632138,-3.6397548305107,2.53374166159966));
#18810=CARTESIAN_POINT('Ctrl Pts',(88.7985382566571,-3.71098670015548,2.42821817914777));
#18811=CARTESIAN_POINT('Ctrl Pts',(88.8042297501004,-3.77754558299305,2.31983584945352));
#18812=CARTESIAN_POINT('Ctrl Pts',(88.8099215937074,-3.84410856080245,2.21144685163973));
#18813=CARTESIAN_POINT('Ctrl Pts',(88.8156134373145,-3.90599777110583,2.10019899691251));
#18814=CARTESIAN_POINT('Ctrl Pts',(88.8213052809215,-3.96297381061829,1.98653657815646));
#18815=CARTESIAN_POINT('Ctrl Pts',(88.8269987566779,-4.01996618814281,1.87284156643705));
#18816=CARTESIAN_POINT('Ctrl Pts',(88.8326922324343,-4.07204241335886,1.75673096999529));
#18817=CARTESIAN_POINT('Ctrl Pts',(88.8383857081907,-4.11901032098851,1.63867110049275));
#18818=CARTESIAN_POINT('Ctrl Pts',(88.8440852364875,-4.16602815860239,1.52048572556064));
#18819=CARTESIAN_POINT('Ctrl Pts',(88.8497847647842,-4.20792668839129,1.40034731138838));
#18820=CARTESIAN_POINT('Ctrl Pts',(88.855484293081,-4.24456283540365,1.2787397453392));
#18821=CARTESIAN_POINT('Ctrl Pts',(88.8611872734499,-4.28122117208105,1.15705852440604));
#18822=CARTESIAN_POINT('Ctrl Pts',(88.8668902538188,-4.31261067806839,1.03390676510222));
#18823=CARTESIAN_POINT('Ctrl Pts',(88.8725932341877,-4.3386392150289,0.909779512746562));
#18824=CARTESIAN_POINT('Ctrl Pts',(88.8783043816994,-4.36470502702142,0.785474499830974));
#18825=CARTESIAN_POINT('Ctrl Pts',(88.884015529211,-4.38539447522944,0.660191597354542));
#18826=CARTESIAN_POINT('Ctrl Pts',(88.8897266767226,-4.40066711891885,0.534432323560671));
#18827=CARTESIAN_POINT('Ctrl Pts',(88.8922294335345,-4.40735994430141,0.479321703758624));
#18828=CARTESIAN_POINT('Ctrl Pts',(88.8947321903464,-4.41301320469446,0.424119621980317));
#18829=CARTESIAN_POINT('Ctrl Pts',(88.8972349471583,-4.41762664990758,0.368868244806094));
#18830=CARTESIAN_POINT('Ctrl Pts',(88.9027593448528,-4.42781002288959,0.246910498362148));
#18831=CARTESIAN_POINT('Ctrl Pts',(88.9082837425472,-4.43294378999581,0.124525430472263));
#18832=CARTESIAN_POINT('Ctrl Pts',(88.9138081402417,-4.43299954096772,0.0020173695596966));
#18833=CARTESIAN_POINT('',(90.1638081402164,-4.43299995951971,0.000599081182435214));
#18834=CARTESIAN_POINT('Ctrl Pts',(88.9138081402808,-4.43299954096812,0.00201736869288152));
#18835=CARTESIAN_POINT('Ctrl Pts',(88.9194545459565,-4.4330565231925,-0.123196319517583));
#18836=CARTESIAN_POINT('Ctrl Pts',(88.9251009516322,-4.42780414529691,-0.248614353895448));
#18837=CARTESIAN_POINT('Ctrl Pts',(88.9307473573079,-4.41721677621254,-0.373744500891365));
#18838=CARTESIAN_POINT('Ctrl Pts',(88.9363873218383,-4.40664148468451,-0.498731905493998));
#18839=CARTESIAN_POINT('Ctrl Pts',(88.9420272863687,-4.39074333915652,-0.623431671623798));
#18840=CARTESIAN_POINT('Ctrl Pts',(88.9476672508991,-4.36954872255428,-0.747350628034997));
#18841=CARTESIAN_POINT('Ctrl Pts',(88.9533022651983,-4.34837270859601,-0.871160820024008));
#18842=CARTESIAN_POINT('Ctrl Pts',(88.9589372794975,-4.32190953918227,-0.994191164384936));
#18843=CARTESIAN_POINT('Ctrl Pts',(88.9645722937967,-4.29023743684232,-1.11595328554407));
#18844=CARTESIAN_POINT('Ctrl Pts',(88.9702041456767,-4.25858310916301,-1.23764707273667));
#18845=CARTESIAN_POINT('Ctrl Pts',(88.9758359975566,-4.22172576483138,-1.35807365737974));
#18846=CARTESIAN_POINT('Ctrl Pts',(88.9814678494366,-4.17979467064512,-1.47675506135806));
#18847=CARTESIAN_POINT('Ctrl Pts',(88.9870981372219,-4.1378752216866,-1.59540350478515));
#18848=CARTESIAN_POINT('Ctrl Pts',(88.9927284250073,-4.09088496036981,-1.71230734581001));
#18849=CARTESIAN_POINT('Ctrl Pts',(88.9983587127926,-4.03900277772549,-1.82700453243165));
#18850=CARTESIAN_POINT('Ctrl Pts',(89.0039887770741,-3.98712265463244,-1.94169716595385));
#18851=CARTESIAN_POINT('Ctrl Pts',(89.0096188413556,-3.93035116527151,-2.05418294677198));
#18852=CARTESIAN_POINT('Ctrl Pts',(89.0152489056372,-3.86891476729876,-2.16402114670296));
#18853=CARTESIAN_POINT('Ctrl Pts',(89.0208800865879,-3.80746618400578,-2.27388113198731));
#18854=CARTESIAN_POINT('Ctrl Pts',(89.0265112675387,-3.74135105259411,-2.38109213569407));
#18855=CARTESIAN_POINT('Ctrl Pts',(89.0321424484895,-3.6708407387347,-2.48523988195218));
#18856=CARTESIAN_POINT('Ctrl Pts',(89.0377792591468,-3.60025993302226,-2.58949174868885));
#18857=CARTESIAN_POINT('Ctrl Pts',(89.0434160698042,-3.52527540145758,-2.69067390452457));
#18858=CARTESIAN_POINT('Ctrl Pts',(89.0490528804616,-3.44620073351959,-2.78840267972347));
#18859=CARTESIAN_POINT('Ctrl Pts',(89.0546927901858,-3.36708259105331,-2.88618518530801));
#18860=CARTESIAN_POINT('Ctrl Pts',(89.0603326999101,-3.28387010488153,-2.98051022352839));
#18861=CARTESIAN_POINT('Ctrl Pts',(89.0659726096343,-3.19691475024118,-3.07102997049693));
#18862=CARTESIAN_POINT('Ctrl Pts',(89.0716207710934,-3.10983217148545,-3.16168215663244));
#18863=CARTESIAN_POINT('Ctrl Pts',(89.0772689325524,-3.01899608510845,-3.24851765287657));
#18864=CARTESIAN_POINT('Ctrl Pts',(89.0829170940115,-2.92479238156857,-3.33122778037144));
#18865=CARTESIAN_POINT('Ctrl Pts',(89.0862173321046,-2.86974886817328,-3.37955556197255));
#18866=CARTESIAN_POINT('Ctrl Pts',(89.0895175701976,-2.8135562087113,-3.42647568460351));
#18867=CARTESIAN_POINT('Ctrl Pts',(89.0928178082907,-2.75629587337804,-3.47193347551464));
#18868=CARTESIAN_POINT('Ctrl Pts',(89.0985282426873,-2.6572177525789,-3.5505895377424));
#18869=CARTESIAN_POINT('Ctrl Pts',(89.104238677084,-2.55461701880162,-3.6251226509496));
#18870=CARTESIAN_POINT('Ctrl Pts',(89.1099491114806,-2.44887108704103,-3.69520221355401));
#18871=CARTESIAN_POINT('Ctrl Pts',(89.115652579348,-2.34325416160057,-3.76519628155511));
#18872=CARTESIAN_POINT('Ctrl Pts',(89.1213560472154,-2.23450000180226,-3.8307473894226));
#18873=CARTESIAN_POINT('Ctrl Pts',(89.1270595150828,-2.12301898023598,-3.89156516193135));
#18874=CARTESIAN_POINT('Ctrl Pts',(89.1327574445841,-2.01164621258168,-3.95232387719699));
#18875=CARTESIAN_POINT('Ctrl Pts',(89.1384553740854,-1.89755220065201,-4.00835821292962));
#18876=CARTESIAN_POINT('Ctrl Pts',(89.1441533035867,-1.78117577892564,-4.05942136819629));
#18877=CARTESIAN_POINT('Ctrl Pts',(89.1498471178977,-1.66488340722561,-4.11044764434706));
#18878=CARTESIAN_POINT('Ctrl Pts',(89.1555409322086,-1.54631227093223,-4.15650972592692));
#18879=CARTESIAN_POINT('Ctrl Pts',(89.1612347465196,-1.42592483029627,-4.19740722093348));
#18880=CARTESIAN_POINT('Ctrl Pts',(89.1669264337978,-1.30558236268251,-4.23828943790156));
#18881=CARTESIAN_POINT('Ctrl Pts',(89.1726181210759,-1.18342531725983,-4.27401077616654));
#18882=CARTESIAN_POINT('Ctrl Pts',(89.1783098083541,-1.05993480737755,-4.30441949676255));
#18883=CARTESIAN_POINT('Ctrl Pts',(89.1840005679819,-0.936464424393002,
-4.33482326124321));
#18884=CARTESIAN_POINT('Ctrl Pts',(89.1896913276098,-0.811661396790677,
-4.35991603489422));
#18885=CARTESIAN_POINT('Ctrl Pts',(89.1953820872377,-0.686020105580647,
-4.37959648994506));
#18886=CARTESIAN_POINT('Ctrl Pts',(89.2010732020358,-0.560370972878362,
-4.39927817328745));
#18887=CARTESIAN_POINT('Ctrl Pts',(89.2067643168339,-0.433883866991581,
-4.41354680440245));
#18888=CARTESIAN_POINT('Ctrl Pts',(89.212455431632,-0.30706090971149,-4.42235260893194));
#18889=CARTESIAN_POINT('Ctrl Pts',(89.2181481843615,-0.180201452148253,
-4.43116094781614));
#18890=CARTESIAN_POINT('Ctrl Pts',(89.2238409370909,-0.0530063490580594,
-4.43450330477294));
#18891=CARTESIAN_POINT('Ctrl Pts',(89.2295336898204,0.0740201563008517,
-4.4323819799811));
#18892=CARTESIAN_POINT('Ctrl Pts',(89.2352325076746,0.20118199716931,-4.43025839510527));
#18893=CARTESIAN_POINT('Ctrl Pts',(89.2409313255287,0.328174482094933,-4.42265951275499));
#18894=CARTESIAN_POINT('Ctrl Pts',(89.2466301433829,0.454496060127244,-4.40963970538737));
#18895=CARTESIAN_POINT('Ctrl Pts',(89.2523324195372,0.580894295799256,-4.39661199701252));
#18896=CARTESIAN_POINT('Ctrl Pts',(89.2580346956914,0.706620419135217,-4.37815686817547));
#18897=CARTESIAN_POINT('Ctrl Pts',(89.2637369718457,0.83118220849259,-4.35437999447515));
#18898=CARTESIAN_POINT('Ctrl Pts',(89.2694474307545,0.955922743761389,-4.33056900100999));
#18899=CARTESIAN_POINT('Ctrl Pts',(89.2751578896633,1.07949522109567,-4.30142110549928));
#18900=CARTESIAN_POINT('Ctrl Pts',(89.2808683485721,1.20142136408789,-4.26709218390149));
#18901=CARTESIAN_POINT('Ctrl Pts',(89.2833791221891,1.2550298302263,-4.25199844940059));
#18902=CARTESIAN_POINT('Ctrl Pts',(89.2858898958061,1.30832027256013,-4.23590376169526));
#18903=CARTESIAN_POINT('Ctrl Pts',(89.2884006694231,1.36125330380707,-4.21882429627904));
#18904=CARTESIAN_POINT('Ctrl Pts',(89.2941122456653,1.48166680570748,-4.17997146293647));
#18905=CARTESIAN_POINT('Ctrl Pts',(89.2998238219076,1.60060131848022,-4.13589934475267));
#18906=CARTESIAN_POINT('Ctrl Pts',(89.3055353981499,1.71757231989815,-4.08673883749864));
#18907=CARTESIAN_POINT('Ctrl Pts',(89.3112400023538,1.83440053650861,-4.03763833976386));
#18908=CARTESIAN_POINT('Ctrl Pts',(89.3169446065577,1.94926964544813,-3.98346196360719));
#18909=CARTESIAN_POINT('Ctrl Pts',(89.3226492107615,2.06171033532708,-3.92439033395067));
#18910=CARTESIAN_POINT('Ctrl Pts',(89.3283482698448,2.17404172802027,-3.8653761244584));
#18911=CARTESIAN_POINT('Ctrl Pts',(89.3340473289281,2.28394904745643,-3.80147631458369));
#18912=CARTESIAN_POINT('Ctrl Pts',(89.3397463880114,2.39098346962001,-3.73291937335966));
#18913=CARTESIAN_POINT('Ctrl Pts',(89.3454413239051,2.4979404538748,-3.66441203212462));
#18914=CARTESIAN_POINT('Ctrl Pts',(89.3511362597987,2.60202834278606,-3.5912544801427));
#18915=CARTESIAN_POINT('Ctrl Pts',(89.3568311956924,2.70282383793958,-3.51372057811454));
#18916=CARTESIAN_POINT('Ctrl Pts',(89.36252398868,2.80358140548796,-3.43621585075551));
#18917=CARTESIAN_POINT('Ctrl Pts',(89.3682167816676,2.90104872678693,-3.35433829062534));
#18918=CARTESIAN_POINT('Ctrl Pts',(89.3739095746552,2.99483265306231,-3.26840425592548));
#18919=CARTESIAN_POINT('Ctrl Pts',(89.3796014297969,3.08860112912376,-3.18248437822748));
#18920=CARTESIAN_POINT('Ctrl Pts',(89.3852932849386,3.178687123026,-3.09250962474938));
#18921=CARTESIAN_POINT('Ctrl Pts',(89.3909851400803,3.26473208148281,-2.99883534661991));
#18922=CARTESIAN_POINT('Ctrl Pts',(89.3966773390632,3.35078223785883,-2.90515540968904));
#18923=CARTESIAN_POINT('Ctrl Pts',(89.4023695380461,3.43279060328041,-2.80777579755594));
#18924=CARTESIAN_POINT('Ctrl Pts',(89.408061737029,3.51043723352108,-2.70708688990747));
#18925=CARTESIAN_POINT('Ctrl Pts',(89.4137555614725,3.58810603648166,-2.60636922960173));
#18926=CARTESIAN_POINT('Ctrl Pts',(89.4194493859159,3.66141038284046,-2.5023407097677));
#18927=CARTESIAN_POINT('Ctrl Pts',(89.4251432103594,3.73007248579902,-2.39542235329913));
#18928=CARTESIAN_POINT('Ctrl Pts',(89.4308430754453,3.79880743315509,-2.2883905659433));
#18929=CARTESIAN_POINT('Ctrl Pts',(89.4365429405311,3.86289008791965,-2.17846315672718));
#18930=CARTESIAN_POINT('Ctrl Pts',(89.442242805617,3.9220874885155,-2.06608778429915));
#18931=CARTESIAN_POINT('Ctrl Pts',(89.4479461164316,3.981320675605,-1.95364447779781));
#18932=CARTESIAN_POINT('Ctrl Pts',(89.4536494272463,4.03566255485428,-1.83875062019934));
#18933=CARTESIAN_POINT('Ctrl Pts',(89.4593527380609,4.08492802804647,-1.72187456154053));
#18934=CARTESIAN_POINT('Ctrl Pts',(89.4650642035028,4.13426394130113,-1.60483139280766));
#18935=CARTESIAN_POINT('Ctrl Pts',(89.4707756689446,4.17850881666604,-1.48580073711594));
#18936=CARTESIAN_POINT('Ctrl Pts',(89.4764871343865,4.21752706231804,-1.36526718213504));
#18937=CARTESIAN_POINT('Ctrl Pts',(89.4789859331095,4.23459776744642,-1.3125330640123));
#18938=CARTESIAN_POINT('Ctrl Pts',(89.4814847318325,4.25066869432302,-1.25951142258196));
#18939=CARTESIAN_POINT('Ctrl Pts',(89.4839835305555,4.26573157368928,-1.20624340049196));
#18940=CARTESIAN_POINT('Ctrl Pts',(89.4896968642443,4.30017182505524,-1.08444968323914));
#18941=CARTESIAN_POINT('Ctrl Pts',(89.4954101979331,4.32944464107065,-0.960992981776088));
#18942=CARTESIAN_POINT('Ctrl Pts',(89.5011235316219,4.35339047025895,-0.836349456542256));
#18943=CARTESIAN_POINT('Ctrl Pts',(89.5068299103414,4.37730714965236,-0.711857662667029));
#18944=CARTESIAN_POINT('Ctrl Pts',(89.512536289061,4.3959096689628,-0.586182307686195));
#18945=CARTESIAN_POINT('Ctrl Pts',(89.5182426677805,4.40908830538804,-0.459814435713356));
#18946=CARTESIAN_POINT('Ctrl Pts',(89.5239435161333,4.4222541696689,-0.333569033824196));
#18947=CARTESIAN_POINT('Ctrl Pts',(89.5296443644861,4.43000656996436,-0.20663284490648));
#18948=CARTESIAN_POINT('Ctrl Pts',(89.5353452128389,4.43228696478374,-0.0795063633183393));
#18949=CARTESIAN_POINT('Ctrl Pts',(89.5410419504645,4.43456571527229,0.0475284508126489));
#18950=CARTESIAN_POINT('Ctrl Pts',(89.5467386880903,4.43138030645747,0.174752887121412));
#18951=CARTESIAN_POINT('Ctrl Pts',(89.5524354257159,4.42272412725664,0.301662550181467));
#18952=CARTESIAN_POINT('Ctrl Pts',(89.5581300321501,4.41407118639619,0.428524735402003));
#18953=CARTESIAN_POINT('Ctrl Pts',(89.5638246385843,4.39995157178336,0.555071984286092));
#18954=CARTESIAN_POINT('Ctrl Pts',(89.5695192450185,4.38041075552766,0.680801448924437));
#18955=CARTESIAN_POINT('Ctrl Pts',(89.5752129203096,4.36087313445245,0.806510355141445));
#18956=CARTESIAN_POINT('Ctrl Pts',(89.5809065956008,4.33591613620271,0.931401349165811));
#18957=CARTESIAN_POINT('Ctrl Pts',(89.5866002708919,4.30563686279154,1.05497877029381));
#18958=CARTESIAN_POINT('Ctrl Pts',(89.5922942947075,4.27535573590846,1.17856375591236));
#18959=CARTESIAN_POINT('Ctrl Pts',(89.5979883185231,4.23975178081076,1.30083462135255));
#18960=CARTESIAN_POINT('Ctrl Pts',(89.6036823423387,4.19897265471482,1.42130842710413));
#18961=CARTESIAN_POINT('Ctrl Pts',(89.6093779942809,4.15818186839686,1.54181668065919));
#18962=CARTESIAN_POINT('Ctrl Pts',(89.6150736462231,4.11221309507761,1.66052647469331));
#18963=CARTESIAN_POINT('Ctrl Pts',(89.6207692981654,4.0612628651163,1.77697297121462));
#18964=CARTESIAN_POINT('Ctrl Pts',(89.6264709847466,4.01025865252979,1.89354284475666));
#18965=CARTESIAN_POINT('Ctrl Pts',(89.6321726713278,3.95426260526756,2.00784426720237));
#18966=CARTESIAN_POINT('Ctrl Pts',(89.637874357909,3.89351827117598,2.11943494168111));
#18967=CARTESIAN_POINT('Ctrl Pts',(89.6435794892293,3.83273723770091,2.23109303494082));
#18968=CARTESIAN_POINT('Ctrl Pts',(89.6492846205497,3.76720240764115,2.3400367764139));
#18969=CARTESIAN_POINT('Ctrl Pts',(89.65498975187,3.69720108618562,2.44585222945047));
#18970=CARTESIAN_POINT('Ctrl Pts',(89.6607030204235,3.62709992179128,2.55181860714937));
#18971=CARTESIAN_POINT('Ctrl Pts',(89.666416288977,3.55251977905433,2.6546474649165));
#18972=CARTESIAN_POINT('Ctrl Pts',(89.6721295575305,3.47378892519854,2.75395706269506));
#18973=CARTESIAN_POINT('Ctrl Pts',(89.6746085022496,3.43962819346187,2.79704675831558));
#18974=CARTESIAN_POINT('Ctrl Pts',(89.6770874469687,3.40468651924392,2.83947436736873));
#18975=CARTESIAN_POINT('Ctrl Pts',(89.6795663916878,3.36899283726742,2.88121090211058));
#18976=CARTESIAN_POINT('Ctrl Pts',(89.6852710062034,3.28685357262487,2.9772561426851));
#18977=CARTESIAN_POINT('Ctrl Pts',(89.6909756207189,3.20047554896026,3.06993611006877));
#18978=CARTESIAN_POINT('Ctrl Pts',(89.6966802352345,3.11016511761852,3.15885452991254));
#18979=CARTESIAN_POINT('Ctrl Pts',(89.7023778793997,3.01996503472333,3.2476643021798));
#18980=CARTESIAN_POINT('Ctrl Pts',(89.7080755235648,2.92584238566442,3.33272139209893));
#18981=CARTESIAN_POINT('Ctrl Pts',(89.71377316773,2.82814359689021,3.41366266572561));
#18982=CARTESIAN_POINT('Ctrl Pts',(89.7194652764114,2.73053972630343,3.49452530174505));
#18983=CARTESIAN_POINT('Ctrl Pts',(89.7251573850928,2.6293669355431,3.57127982403108));
#18984=CARTESIAN_POINT('Ctrl Pts',(89.7308494937743,2.52500794957209,3.64360039721671));
#18985=CARTESIAN_POINT('Ctrl Pts',(89.736537496815,2.4207242363198,3.71586880655547));
#18986=CARTESIAN_POINT('Ctrl Pts',(89.7422254998558,2.31325922946158,3.78370940462262));
#18987=CARTESIAN_POINT('Ctrl Pts',(89.7479135028966,2.20302774130567,3.84683737257473));
#18988=CARTESIAN_POINT('Ctrl Pts',(89.7535994139857,2.09283679443274,3.90994212312448));
#18989=CARTESIAN_POINT('Ctrl Pts',(89.7592853250749,1.97988173575953,3.96833749078323));
#18990=CARTESIAN_POINT('Ctrl Pts',(89.764971236164,1.86460500917239,4.02178283349179));
#18991=CARTESIAN_POINT('Ctrl Pts',(89.7706562430049,1.74934661540412,4.07521967662011));
#18992=CARTESIAN_POINT('Ctrl Pts',(89.7763412498458,1.63176765101383,4.12370789224967));
#18993=CARTESIAN_POINT('Ctrl Pts',(89.7820262566867,1.5123332276658,4.16705378037024));
#18994=CARTESIAN_POINT('Ctrl Pts',(89.7877116480865,1.39289072524838,4.21040260059722));
#18995=CARTESIAN_POINT('Ctrl Pts',(89.7933970394862,1.27159289042968,4.2486082649287));
#18996=CARTESIAN_POINT('Ctrl Pts',(89.799082430886,1.14892228474801,4.28152619793566));
#18997=CARTESIAN_POINT('Ctrl Pts',(89.804769495616,1.02621557452629,4.31445381938285));
#18998=CARTESIAN_POINT('Ctrl Pts',(89.8104565603461,0.902135676053021,4.34209050993948));
#18999=CARTESIAN_POINT('Ctrl Pts',(89.8161436250761,0.777177172513956,4.36434240665455));
#19000=CARTESIAN_POINT('Ctrl Pts',(89.8218368387783,0.652083561253556,4.38661836258108));
#19001=CARTESIAN_POINT('Ctrl Pts',(89.8275300524805,0.526109842569052,4.40349783003496));
#19002=CARTESIAN_POINT('Ctrl Pts',(89.8332232661827,0.399757893981526,4.41493857558624));
#19003=CARTESIAN_POINT('Ctrl Pts',(89.838919978335,0.273328302781571,4.4263863514159));
#19004=CARTESIAN_POINT('Ctrl Pts',(89.8446166904872,0.146520417739216,4.43238872920634));
#19005=CARTESIAN_POINT('Ctrl Pts',(89.8503134026395,0.019836724045662,4.43295561723543));
#19006=CARTESIAN_POINT('Ctrl Pts',(89.8560184073785,-0.107031380496429,
4.43352333047176));
#19007=CARTESIAN_POINT('Ctrl Pts',(89.8617234121176,-0.233774533772461,
4.42863977056217));
#19008=CARTESIAN_POINT('Ctrl Pts',(89.8674284168566,-0.35989438068452,4.41836678363756));
#19009=CARTESIAN_POINT('Ctrl Pts',(89.8700020288445,-0.416788908343833,
4.41373248734688));
#19010=CARTESIAN_POINT('Ctrl Pts',(89.8725756408324,-0.473556712224774,
4.40800211356086));
#19011=CARTESIAN_POINT('Ctrl Pts',(89.8751492528202,-0.530152790862976,
4.40118472894972));
#19012=CARTESIAN_POINT('Ctrl Pts',(89.8808663150511,-0.655876211923623,
4.38604048333019));
#19013=CARTESIAN_POINT('Ctrl Pts',(89.886583377282,-0.781143059404232,4.36548164320263));
#19014=CARTESIAN_POINT('Ctrl Pts',(89.8923004395129,-0.905452013692984,
4.33954440591398));
#19015=CARTESIAN_POINT('Ctrl Pts',(89.8980104951791,-1.02960862072852,4.31363895609293));
#19016=CARTESIAN_POINT('Ctrl Pts',(89.9037205508453,-1.15280928364401,4.2823683039651));
#19017=CARTESIAN_POINT('Ctrl Pts',(89.9094306065115,-1.27455813693656,4.24582036308283));
#19018=CARTESIAN_POINT('Ctrl Pts',(89.915135076565,-1.39618789472747,4.20930817362847));
#19019=CARTESIAN_POINT('Ctrl Pts',(89.9208395466184,-1.51636828961105,4.1675290818621));
#19020=CARTESIAN_POINT('Ctrl Pts',(89.9265440166719,-1.63461443897412,4.12062187489914));
#19021=CARTESIAN_POINT('Ctrl Pts',(89.9322443170708,-1.75277415689164,4.0737489545301));
#19022=CARTESIAN_POINT('Ctrl Pts',(89.9379446174698,-1.86900207437685,4.02175552597497));
#19023=CARTESIAN_POINT('Ctrl Pts',(89.9436449178687,-1.98282969524079,3.96482980715078));
#19024=CARTESIAN_POINT('Ctrl Pts',(89.9493429872033,-2.09661276463729,3.90792636872119));
#19025=CARTESIAN_POINT('Ctrl Pts',(89.9550410565379,-2.20799705008679,3.84609465699794));
#19026=CARTESIAN_POINT('Ctrl Pts',(89.9607391258725,-2.3165355321143,3.77957036294496));
#19027=CARTESIAN_POINT('Ctrl Pts',(89.9664362008577,-2.42505507348567,3.71305767780483));
#19028=CARTESIAN_POINT('Ctrl Pts',(89.9721332758429,-2.53072945987447,3.64185424734687));
#19029=CARTESIAN_POINT('Ctrl Pts',(89.9778303508282,-2.63313816388875,3.56624065506979));
#19030=CARTESIAN_POINT('Ctrl Pts',(89.9835277076911,-2.735551934843,3.49062332161136));
#19031=CARTESIAN_POINT('Ctrl Pts',(89.9892250645541,-2.83469938168904,3.41059562899386));
#19032=CARTESIAN_POINT('Ctrl Pts',(89.9949224214171,-2.93019115869967,3.3264799373329));
#19033=CARTESIAN_POINT('Ctrl Pts',(90.0006213362723,-3.02570904877428,3.24234124349827));
#19034=CARTESIAN_POINT('Ctrl Pts',(90.0063202511275,-3.11756898153019,3.15411258987488));
#19035=CARTESIAN_POINT('Ctrl Pts',(90.0120191659827,-3.20541710812029,3.06215449691386));
#19036=CARTESIAN_POINT('Ctrl Pts',(90.0177239928781,-3.29335636814127,2.97010100685293));
#19037=CARTESIAN_POINT('Ctrl Pts',(90.0234288197736,-3.37727523692711,2.87431064087765));
#19038=CARTESIAN_POINT('Ctrl Pts',(90.0291336466691,-3.45685875146728,2.77517865594344));
#19039=CARTESIAN_POINT('Ctrl Pts',(90.0348418523481,-3.53648940073688,2.67598795835606));
#19040=CARTESIAN_POINT('Ctrl Pts',(90.0405500580272,-3.61177934480988,2.57345201936962));
#19041=CARTESIAN_POINT('Ctrl Pts',(90.0462582637062,-3.68245661183773,2.46799560411533));
#19042=CARTESIAN_POINT('Ctrl Pts',(90.0519744799272,-3.75323306296053,2.36239119786559));
#19043=CARTESIAN_POINT('Ctrl Pts',(90.0576906961483,-3.81938370456455,2.25385847099838));
#19044=CARTESIAN_POINT('Ctrl Pts',(90.0634069123693,-3.88068202871538,2.14284763620876));
#19045=CARTESIAN_POINT('Ctrl Pts',(90.0658486462304,-3.90686616659947,2.09542834628483));
#19046=CARTESIAN_POINT('Ctrl Pts',(90.0682903800915,-3.93216552110533,2.04755715069785));
#19047=CARTESIAN_POINT('Ctrl Pts',(90.0707321139525,-3.95656513489585,1.99927020017969));
#19048=CARTESIAN_POINT('Ctrl Pts',(90.0767804072464,-4.01700416259418,1.87966107993336));
#19049=CARTESIAN_POINT('Ctrl Pts',(90.0828287005402,-4.07208307882196,1.7571757525736));
#19050=CARTESIAN_POINT('Ctrl Pts',(90.0888769938341,-4.12153699335669,1.63230567369972));
#19051=CARTESIAN_POINT('Ctrl Pts',(90.0951212560326,-4.1725932490797,1.50338971751872));
#19052=CARTESIAN_POINT('Ctrl Pts',(90.1013655182312,-4.21765361423013,1.37193212879298));
#19053=CARTESIAN_POINT('Ctrl Pts',(90.1076097804297,-4.25647749947866,1.23850244102784));
#19054=CARTESIAN_POINT('Ctrl Pts',(90.113632853541,-4.29392613502294,1.10979920290736));
#19055=CARTESIAN_POINT('Ctrl Pts',(90.1196559266522,-4.32557242099588,0.979261542044126));
#19056=CARTESIAN_POINT('Ctrl Pts',(90.1256789997635,-4.35124866791305,0.847421990501147));
#19057=CARTESIAN_POINT('Ctrl Pts',(90.1316932308378,-4.37688722139333,0.715775983047038));
#19058=CARTESIAN_POINT('Ctrl Pts',(90.137707461912,-4.39657313467367,0.582832213013575));
#19059=CARTESIAN_POINT('Ctrl Pts',(90.1437216929862,-4.41018873685979,0.449137290007243));
#19060=CARTESIAN_POINT('Ctrl Pts',(90.1497248105176,-4.42377917912487,0.315689418410002));
#19061=CARTESIAN_POINT('Ctrl Pts',(90.1557279280489,-4.43132164108185,0.181493486475357));
#19062=CARTESIAN_POINT('Ctrl Pts',(90.1617310455803,-4.43274972705193,0.0471047483914331));
#19063=CARTESIAN_POINT('Ctrl Pts',(90.162423410459,-4.43291443423355,0.0316051280925057));
#19064=CARTESIAN_POINT('Ctrl Pts',(90.1631157753377,-4.43299786430703,0.0161029527467754));
#19065=CARTESIAN_POINT('Ctrl Pts',(90.1638081402164,-4.43299995951971,0.000599081182447127));
#19066=CARTESIAN_POINT('',(90.4430005297901,-0.73483653948465,-4.3716706486466));
#19067=CARTESIAN_POINT('Ctrl Pts',(90.1638081402416,-4.43299995951978,0.000599080619067216));
#19068=CARTESIAN_POINT('Ctrl Pts',(90.1697491429294,-4.43301793797712,-0.13243560306544));
#19069=CARTESIAN_POINT('Ctrl Pts',(90.1756901456173,-4.42704301383578,-0.265377958426872));
#19070=CARTESIAN_POINT('Ctrl Pts',(90.1816311483051,-4.41512607119674,-0.39768175145319));
#19071=CARTESIAN_POINT('Ctrl Pts',(90.1875786320771,-4.40319612827599,-0.530129875675138));
#19072=CARTESIAN_POINT('Ctrl Pts',(90.1935261158492,-4.38531126751376,-0.661937704319379));
#19073=CARTESIAN_POINT('Ctrl Pts',(90.1994735996212,-4.36157388853184,-0.792566851992466));
#19074=CARTESIAN_POINT('Ctrl Pts',(90.2054333755474,-4.33778744955514,-0.923465981676113));
#19075=CARTESIAN_POINT('Ctrl Pts',(90.2113931514737,-4.30812437494094,-1.05318122000487));
#19076=CARTESIAN_POINT('Ctrl Pts',(90.2173529273999,-4.27273795706517,-1.18118556977917));
#19077=CARTESIAN_POINT('Ctrl Pts',(90.2233190998679,-4.23731355945599,-1.30932730478125));
#19078=CARTESIAN_POINT('Ctrl Pts',(90.229285272336,-4.19615366813219,-1.43575415893636));
#19079=CARTESIAN_POINT('Ctrl Pts',(90.235251444804,-4.14946055740378,-1.55995707714998));
#19080=CARTESIAN_POINT('Ctrl Pts',(90.2412300433691,-4.10267019619687,-1.68441868006116));
#19081=CARTESIAN_POINT('Ctrl Pts',(90.2472086419342,-4.05032370960136,-1.80664676772079));
#19082=CARTESIAN_POINT('Ctrl Pts',(90.2531872404993,-3.99267099489296,-1.92615350544563));
#19083=CARTESIAN_POINT('Ctrl Pts',(90.2575631520279,-3.95047328313869,-2.0136239896494));
#19084=CARTESIAN_POINT('Ctrl Pts',(90.2619390635564,-3.90543389479463,-2.09963708311972));
#19085=CARTESIAN_POINT('Ctrl Pts',(90.266314975085,-3.85766565530893,-2.1840111473731));
#19086=CARTESIAN_POINT('Ctrl Pts',(90.2719042780933,-3.79665181558217,-2.29178119895709));
#19087=CARTESIAN_POINT('Ctrl Pts',(90.2774935811017,-3.73100228864556,-2.39719699742482));
#19088=CARTESIAN_POINT('Ctrl Pts',(90.2830828841101,-3.66092610540627,-2.4998218038002));
#19089=CARTESIAN_POINT('Ctrl Pts',(90.288665249716,-3.59093690021812,-2.60231923300912));
#19090=CARTESIAN_POINT('Ctrl Pts',(90.294247615322,-3.51653219252369,-2.70203221462205));
#19091=CARTESIAN_POINT('Ctrl Pts',(90.2998299809279,-3.4379671796562,-2.79854795771071));
#19092=CARTESIAN_POINT('Ctrl Pts',(90.3054069451015,-3.35947818538567,-2.89497031328366));
#19093=CARTESIAN_POINT('Ctrl Pts',(90.3109839092751,-3.27683715086819,-2.9882012592045));
#19094=CARTESIAN_POINT('Ctrl Pts',(90.3165608734487,-3.19034249513677,-3.07785700832974));
#19095=CARTESIAN_POINT('Ctrl Pts',(90.3221341145495,-3.10390558155529,-3.16745290502057));
#19096=CARTESIAN_POINT('Ctrl Pts',(90.3277073556503,-3.0136204505536,-3.25347805099511));
#19097=CARTESIAN_POINT('Ctrl Pts',(90.3332805967511,-2.91982526417337,-3.33558232197841));
#19098=CARTESIAN_POINT('Ctrl Pts',(90.3388519367764,-2.82606207205449,-3.41765858656176));
#19099=CARTESIAN_POINT('Ctrl Pts',(90.3444232768016,-2.7287915173788,-3.49581635919019));
#19100=CARTESIAN_POINT('Ctrl Pts',(90.3499946168269,-2.62838755126709,-3.56974339138602));
#19101=CARTESIAN_POINT('Ctrl Pts',(90.3555654327219,-2.52799303077463,-3.64366346881079));
#19102=CARTESIAN_POINT('Ctrl Pts',(90.3611362486169,-2.42446602116187,-3.71335334986336));
#19103=CARTESIAN_POINT('Ctrl Pts',(90.366707064512,-2.31821176461007,-3.77854247222702));
#19104=CARTESIAN_POINT('Ctrl Pts',(90.3722787325905,-2.21194125404261,-3.84374156675602));
#19105=CARTESIAN_POINT('Ctrl Pts',(90.3778504006691,-2.10294302376899,-3.90443831706234));
#19106=CARTESIAN_POINT('Ctrl Pts',(90.3834220687476,-1.99164869650006,-3.96040710908988));
#19107=CARTESIAN_POINT('Ctrl Pts',(90.3889990417093,-1.88024840394588,-4.01642918998808));
#19108=CARTESIAN_POINT('Ctrl Pts',(90.394576014671,-1.76654802370243,-4.06771413882168));
#19109=CARTESIAN_POINT('Ctrl Pts',(90.4001529876326,-1.65100105872653,-4.1140836773313));
#19110=CARTESIAN_POINT('Ctrl Pts',(90.4057328907888,-1.53539338427969,-4.16047757883611));
#19111=CARTESIAN_POINT('Ctrl Pts',(90.4113127939449,-1.4179375872935,-4.2019507919376));
#19112=CARTESIAN_POINT('Ctrl Pts',(90.4168926971011,-1.29910262865179,-4.23837484895213));
#19113=CARTESIAN_POINT('Ctrl Pts',(90.4224806058266,-1.18009717574056,-4.27485116409899));
#19114=CARTESIAN_POINT('Ctrl Pts',(90.4280685145522,-1.05970901435191,-4.30626375853715));
#19115=CARTESIAN_POINT('Ctrl Pts',(90.4336564232778,-0.938417771461562,
-4.33253518003087));
#19116=CARTESIAN_POINT('Ctrl Pts',(90.4367711254486,-0.870809992580504,
-4.34717887905574));
#19117=CARTESIAN_POINT('Ctrl Pts',(90.4398858276193,-0.802921749507619,
-4.36022616800192));
#19118=CARTESIAN_POINT('Ctrl Pts',(90.4430005297901,-0.734836539484649,
-4.3716706486466));
#19119=CARTESIAN_POINT('',(90.4430005297901,-3.92880598357857,-2.05328335682078));
#19120=CARTESIAN_POINT('Origin',(90.4430005297901,0.,0.));
#19121=CARTESIAN_POINT('',(90.3471929085019,-4.43299985814068,-0.00112148327145838));
#19122=CARTESIAN_POINT('Ctrl Pts',(90.4430005297901,-3.92880598357866,-2.05328335682061));
#19123=CARTESIAN_POINT('Ctrl Pts',(90.4110646596396,-4.25841379539657,-1.42260316404407));
#19124=CARTESIAN_POINT('Ctrl Pts',(90.379128789489,-4.43043959253044,-0.713287670544325));
#19125=CARTESIAN_POINT('Ctrl Pts',(90.3471929193385,-4.43169289886078,-0.00112139428608522));
#19126=CARTESIAN_POINT('',(89.0971929193785,-4.43299919376221,0.0026735937699673));
#19127=CARTESIAN_POINT('Ctrl Pts',(90.3471929085019,-4.43299985814068,-0.00112148327145838));
#19128=CARTESIAN_POINT('Ctrl Pts',(90.3465316387426,-4.43300358982262,0.0136291117150349));
#19129=CARTESIAN_POINT('Ctrl Pts',(90.3458703689832,-4.43293369846719,0.0283807072529051));
#19130=CARTESIAN_POINT('Ctrl Pts',(90.3452090992239,-4.4327901571182,0.0431326205558783));
#19131=CARTESIAN_POINT('Ctrl Pts',(90.3394423924397,-4.43153838224206,0.171778997204193));
#19132=CARTESIAN_POINT('Ctrl Pts',(90.3336756856555,-4.42468163753682,0.300407073394231));
#19133=CARTESIAN_POINT('Ctrl Pts',(90.3279089788713,-4.41224152195584,0.428501752538767));
#19134=CARTESIAN_POINT('Ctrl Pts',(90.3221427954218,-4.39980253532841,0.556584806956697));
#19135=CARTESIAN_POINT('Ctrl Pts',(90.3163766119723,-4.3817812253595,0.684134176035194));
#19136=CARTESIAN_POINT('Ctrl Pts',(90.3106104285228,-4.35825108459229,0.810639552236455));
#19137=CARTESIAN_POINT('Ctrl Pts',(90.3048414539242,-4.33470955394638,0.937206163978292));
#19138=CARTESIAN_POINT('Ctrl Pts',(90.2990724793256,-4.30565393347754,1.06272739217585));
#19139=CARTESIAN_POINT('Ctrl Pts',(90.2933035047271,-4.27120895910102,1.18670258603206));
#19140=CARTESIAN_POINT('Ctrl Pts',(90.2875331119772,-4.23675551732975,1.31070825594247));
#19141=CARTESIAN_POINT('Ctrl Pts',(90.2817627192273,-4.19691019416052,1.43316676394973));
#19142=CARTESIAN_POINT('Ctrl Pts',(90.2759923264775,-4.15184747744202,1.55359310118779));
#19143=CARTESIAN_POINT('Ctrl Pts',(90.2702164523881,-4.10674195530944,1.67413383231083));
#19144=CARTESIAN_POINT('Ctrl Pts',(90.2644405782986,-4.05640928324267,1.79263817711511));
#19145=CARTESIAN_POINT('Ctrl Pts',(90.2586647042092,-4.0010720782519,1.90864119850564));
#19146=CARTESIAN_POINT('Ctrl Pts',(90.2549156923587,-3.96515373341394,1.98393659019094));
#19147=CARTESIAN_POINT('Ctrl Pts',(90.2511666805082,-3.9271279119575,2.05817860910029));
#19148=CARTESIAN_POINT('Ctrl Pts',(90.2474176686577,-3.88706567518093,2.13124598224377));
#19149=CARTESIAN_POINT('Ctrl Pts',(90.2416408381269,-3.82533400780438,2.24383507206739));
#19150=CARTESIAN_POINT('Ctrl Pts',(90.235864007596,-3.75864455320898,2.35385355122844));
#19151=CARTESIAN_POINT('Ctrl Pts',(90.2300871770651,-3.68723787993225,2.4608465650651));
#19152=CARTESIAN_POINT('Ctrl Pts',(90.2243153194889,-3.61589267672022,2.56774747452018));
#19153=CARTESIAN_POINT('Ctrl Pts',(90.2185434619126,-3.53983855315819,2.67162778396671));
#19154=CARTESIAN_POINT('Ctrl Pts',(90.2127716043364,-3.45936110806888,2.7720587518991));
#19155=CARTESIAN_POINT('Ctrl Pts',(90.2070034129191,-3.37893478050945,2.87242592825613));
#19156=CARTESIAN_POINT('Ctrl Pts',(90.2012352215017,-3.29409096713205,2.96934782523667));
#19157=CARTESIAN_POINT('Ctrl Pts',(90.1954670300844,-3.20515734868601,3.06242638608083));
#19158=CARTESIAN_POINT('Ctrl Pts',(90.1894823541444,-3.1128859852621,3.15899825468006));
#19159=CARTESIAN_POINT('Ctrl Pts',(90.1834976782045,-3.01621208747336,3.25143231607391));
#19160=CARTESIAN_POINT('Ctrl Pts',(90.1775130022645,-2.91554609764722,3.33932327762588));
#19161=CARTESIAN_POINT('Ctrl Pts',(90.1717470295916,-2.81855883346521,3.42400236260755));
#19162=CARTESIAN_POINT('Ctrl Pts',(90.1659810569186,-2.71786644577177,3.50446429911993));
#19163=CARTESIAN_POINT('Ctrl Pts',(90.1602150842457,-2.61387159739403,3.58038605074045));
#19164=CARTESIAN_POINT('Ctrl Pts',(90.1544486145709,-2.50986778511079,3.65631434648711));
#19165=CARTESIAN_POINT('Ctrl Pts',(90.148682144896,-2.40256125726051,3.72770144985256));
#19166=CARTESIAN_POINT('Ctrl Pts',(90.1429156752212,-2.29238516605498,3.79426662880339));
#19167=CARTESIAN_POINT('Ctrl Pts',(90.1371475287528,-2.18217703747118,3.86085116380321));
#19168=CARTESIAN_POINT('Ctrl Pts',(90.1313793822843,-2.06909801481257,3.92261078270365));
#19169=CARTESIAN_POINT('Ctrl Pts',(90.1256112358158,-1.95360712907898,3.97931001370989));
#19170=CARTESIAN_POINT('Ctrl Pts',(90.1198402318251,-1.83805902951072,4.03603733334328));
#19171=CARTESIAN_POINT('Ctrl Pts',(90.1140692278344,-1.72009703434979,4.08769910332605));
#19172=CARTESIAN_POINT('Ctrl Pts',(90.1082982238436,-1.60020115215999,4.13410755455465));
#19173=CARTESIAN_POINT('Ctrl Pts',(90.102519848168,-1.48015211903506,4.18057528636549));
#19174=CARTESIAN_POINT('Ctrl Pts',(90.0967414724924,-1.35816462678385,4.22177616058313));
#19175=CARTESIAN_POINT('Ctrl Pts',(90.0909630968168,-1.23473538928447,4.25757178664653));
#19176=CARTESIAN_POINT('Ctrl Pts',(90.0851803838934,-1.1112135058181,4.29339428090144));
#19177=CARTESIAN_POINT('Ctrl Pts',(90.0793976709699,-0.986248094925947,
4.32380335007161));
#19178=CARTESIAN_POINT('Ctrl Pts',(90.0736149580464,-0.860346192411113,
4.34871169764146));
#19179=CARTESIAN_POINT('Ctrl Pts',(90.0678235788045,-0.734255605799044,
4.37365737434599));
#19180=CARTESIAN_POINT('Ctrl Pts',(90.0620321995627,-0.607226105872629,
4.39308581009496));
#19181=CARTESIAN_POINT('Ctrl Pts',(90.0562408203209,-0.479770447597029,
4.40696146087217));
#19182=CARTESIAN_POINT('Ctrl Pts',(90.054772149389,-0.447448195403114,4.4104802711772));
#19183=CARTESIAN_POINT('Ctrl Pts',(90.0533034784572,-0.415098537276401,
4.41364223814709));
#19184=CARTESIAN_POINT('Ctrl Pts',(90.0518348075254,-0.38272982472858,4.41644731444441));
#19185=CARTESIAN_POINT('Ctrl Pts',(90.0461769990587,-0.258034787916835,
4.42725340046459));
#19186=CARTESIAN_POINT('Ctrl Pts',(90.0405191905921,-0.132649939074645,
4.43279429414113));
#19187=CARTESIAN_POINT('Ctrl Pts',(90.0348613821254,-0.00706243780706909,
4.43299437423196));
#19188=CARTESIAN_POINT('Ctrl Pts',(90.0292112553074,0.118354552376854,4.43319418267257));
#19189=CARTESIAN_POINT('Ctrl Pts',(90.0235611284893,0.243973244670051,4.42806759582563));
#19190=CARTESIAN_POINT('Ctrl Pts',(90.0179110016713,0.369300054675269,4.4175905728821));
#19191=CARTESIAN_POINT('Ctrl Pts',(90.0122670675232,0.494489503590794,4.40712503299865));
#19192=CARTESIAN_POINT('Ctrl Pts',(90.0066231333752,0.619387303110374,4.39132075383049));
#19193=CARTESIAN_POINT('Ctrl Pts',(90.0009791992271,0.74349914601596,4.37020571825555));
#19194=CARTESIAN_POINT('Ctrl Pts',(89.9953399751504,0.867507413008013,4.3491083039571));
#19195=CARTESIAN_POINT('Ctrl Pts',(89.9897007510737,0.990730627962674,4.32270901803345));
#19196=CARTESIAN_POINT('Ctrl Pts',(89.984061526997,1.11267947801103,4.29108766855364));
#19197=CARTESIAN_POINT('Ctrl Pts',(89.9784251344186,1.23456709659216,4.25948219639963));
#19198=CARTESIAN_POINT('Ctrl Pts',(89.9727887418402,1.35518122870269,4.22265997654248));
#19199=CARTESIAN_POINT('Ctrl Pts',(89.9671523492618,1.47404311377501,4.18075183414807));
#19200=CARTESIAN_POINT('Ctrl Pts',(89.961517313954,1.59287637633131,4.13885378343676));
#19201=CARTESIAN_POINT('Ctrl Pts',(89.9558822786462,1.70995784635137,4.09187238064173));
#19202=CARTESIAN_POINT('Ctrl Pts',(89.9502472433383,1.82482485428986,4.03998802611666));
#19203=CARTESIAN_POINT('Ctrl Pts',(89.9446122312962,1.93969138796984,3.98810388580973));
#19204=CARTESIAN_POINT('Ctrl Pts',(89.9389772192541,2.05234310615974,3.93131700221962));
#19205=CARTESIAN_POINT('Ctrl Pts',(89.933342207212,2.16233880620666,3.86985527987453));
#19206=CARTESIAN_POINT('Ctrl Pts',(89.9277058847034,2.27236008662219,3.80837926412058));
#19207=CARTESIAN_POINT('Ctrl Pts',(89.9220695621947,2.37972376492447,3.74222644710263));
#19208=CARTESIAN_POINT('Ctrl Pts',(89.916433239686,2.4840152113769,3.67166956977996));
#19209=CARTESIAN_POINT('Ctrl Pts',(89.9107910563432,2.58841510351825,3.60103932508701));
#19210=CARTESIAN_POINT('Ctrl Pts',(89.9051488730003,2.6897360476216,3.52599610595527));
#19211=CARTESIAN_POINT('Ctrl Pts',(89.8995066896574,2.7875941097298,3.44685480973593));
#19212=CARTESIAN_POINT('Ctrl Pts',(89.8938612494158,2.88550865951021,3.36766782992647));
#19213=CARTESIAN_POINT('Ctrl Pts',(89.8882158091741,2.97995604176652,3.28437833213289));
#19214=CARTESIAN_POINT('Ctrl Pts',(89.8825703689325,3.07058825043254,3.19733901804385));
#19215=CARTESIAN_POINT('Ctrl Pts',(89.8769165617387,3.16135478260924,3.11017070537465));
#19216=CARTESIAN_POINT('Ctrl Pts',(89.8712627545449,3.24829457044237,3.01924177439788));
#19217=CARTESIAN_POINT('Ctrl Pts',(89.8656089473511,3.33109881978181,2.9249392562664));
#19218=CARTESIAN_POINT('Ctrl Pts',(89.8624899470317,3.37677892016065,2.87291597813046));
#19219=CARTESIAN_POINT('Ctrl Pts',(89.8593709467124,3.42120118246359,2.81986655700101));
#19220=CARTESIAN_POINT('Ctrl Pts',(89.856251946393,3.46431945908368,2.76585966480843));
#19221=CARTESIAN_POINT('Ctrl Pts',(89.8505264815675,3.54347051738678,2.66672066835993));
#19222=CARTESIAN_POINT('Ctrl Pts',(89.8448010167419,3.61847966456172,2.56403472814382));
#19223=CARTESIAN_POINT('Ctrl Pts',(89.8390755519164,3.68901516440634,2.45818146538861));
#19224=CARTESIAN_POINT('Ctrl Pts',(89.8333569411806,3.75946622453167,2.35245492208405));
#19225=CARTESIAN_POINT('Ctrl Pts',(89.8276383304447,3.8254540750884,2.2435689281578));
#19226=CARTESIAN_POINT('Ctrl Pts',(89.8219197197089,3.8866872680214,2.13193599355148));
#19227=CARTESIAN_POINT('Ctrl Pts',(89.8162065547643,3.94786214903203,2.0204093661734));
#19228=CARTESIAN_POINT('Ctrl Pts',(89.8104933898197,4.00429119343185,1.90614135001187));
#19229=CARTESIAN_POINT('Ctrl Pts',(89.8047802248751,4.05572656226878,1.78957286862185));
#19230=CARTESIAN_POINT('Ctrl Pts',(89.7987755940578,4.10978598533994,1.66705746735772));
#19231=CARTESIAN_POINT('Ctrl Pts',(89.7927709632405,4.15832853903692,1.54200106594889));
#19232=CARTESIAN_POINT('Ctrl Pts',(89.7867663324233,4.20112131672355,1.41494476293989));
#19233=CARTESIAN_POINT('Ctrl Pts',(89.7810593649033,4.2417927584458,1.29418693176757));
#19234=CARTESIAN_POINT('Ctrl Pts',(89.7753523973833,4.27727062392836,1.17162312913266));
#19235=CARTESIAN_POINT('Ctrl Pts',(89.7696454298633,4.30740471981902,1.04773736197618));
#19236=CARTESIAN_POINT('Ctrl Pts',(89.7639392990392,4.3375343977634,0.923869757656485));
#19237=CARTESIAN_POINT('Ctrl Pts',(89.7582331682152,4.36232177096677,0.798680959789409));
#19238=CARTESIAN_POINT('Ctrl Pts',(89.7525270373911,4.3816671215063,0.672667998577801));
#19239=CARTESIAN_POINT('Ctrl Pts',(89.7468204779354,4.40101392522505,0.54664557155599));
#19240=CARTESIAN_POINT('Ctrl Pts',(89.7411139184796,4.41491783292752,0.419799250219));
#19241=CARTESIAN_POINT('Ctrl Pts',(89.7354073590239,4.42333071143737,0.2926335887334));
#19242=CARTESIAN_POINT('Ctrl Pts',(89.7296991056221,4.43174608724209,0.165430179150732));
#19243=CARTESIAN_POINT('Ctrl Pts',(89.7239908522204,4.4346671647022,0.0379076365427575));
#19244=CARTESIAN_POINT('Ctrl Pts',(89.7182825988186,4.43209789078656,-0.089427548805418));
#19245=CARTESIAN_POINT('Ctrl Pts',(89.7125683489679,4.42952591788072,-0.216896498177392));
#19246=CARTESIAN_POINT('Ctrl Pts',(89.7068540991172,4.42145208632748,-0.344177300343669));
#19247=CARTESIAN_POINT('Ctrl Pts',(89.7011398492665,4.40793240160502,-0.470766335755432));
#19248=CARTESIAN_POINT('Ctrl Pts',(89.6954221188922,4.3944044821041,-0.597432475972821));
#19249=CARTESIAN_POINT('Ctrl Pts',(89.6897043885178,4.37542415965407,-0.72340561826698));
#19250=CARTESIAN_POINT('Ctrl Pts',(89.6839866581435,4.35109871531903,-0.848191587761348));
#19251=CARTESIAN_POINT('Ctrl Pts',(89.6782610095774,4.32673958392263,-0.973150366950498));
#19252=CARTESIAN_POINT('Ctrl Pts',(89.6725353610113,4.29702064340578,-1.0969183058555));
#19253=CARTESIAN_POINT('Ctrl Pts',(89.6668097124451,4.26209932403515,-1.21901532068268));
#19254=CARTESIAN_POINT('Ctrl Pts',(89.664762836717,4.24961521848984,-1.26266407300195));
#19255=CARTESIAN_POINT('Ctrl Pts',(89.6627159609888,4.23646669626051,-1.30609945691691));
#19256=CARTESIAN_POINT('Ctrl Pts',(89.6606690852607,4.22266243405317,-1.34930017714228));
#19257=CARTESIAN_POINT('Ctrl Pts',(89.6549528626141,4.18411185906552,-1.46994498811108));
#19258=CARTESIAN_POINT('Ctrl Pts',(89.6492366399676,4.14032878566903,-1.58911792253836));
#19259=CARTESIAN_POINT('Ctrl Pts',(89.643520417321,4.09144408506085,-1.70633358368772));
#19260=CARTESIAN_POINT('Ctrl Pts',(89.6378110422421,4.04261794432972,-1.8234088300525));
#19261=CARTESIAN_POINT('Ctrl Pts',(89.6321016671633,3.98870248744607,-1.93853110344308));
#19262=CARTESIAN_POINT('Ctrl Pts',(89.6263922920844,3.92987831959161,-2.05123021457949));
#19263=CARTESIAN_POINT('Ctrl Pts',(89.6206883442447,3.87111006903579,-2.16382219577112));
#19264=CARTESIAN_POINT('Ctrl Pts',(89.614984396405,3.80744257623814,-2.27399524723275));
#19265=CARTESIAN_POINT('Ctrl Pts',(89.6092804485654,3.73910429903609,-2.38129965374579));
#19266=CARTESIAN_POINT('Ctrl Pts',(89.6035805124916,3.67081408629359,-2.48852858969508));
#19267=CARTESIAN_POINT('Ctrl Pts',(89.5978805764179,3.59785984110271,-2.59289256170049));
#19268=CARTESIAN_POINT('Ctrl Pts',(89.5921806403441,3.52051542744002,-2.69396735784916));
#19269=CARTESIAN_POINT('Ctrl Pts',(89.5864826996908,3.44319809033185,-2.79500676996558));
#19270=CARTESIAN_POINT('Ctrl Pts',(89.5807847590376,3.36149388194526,-2.89275897963081));
#19271=CARTESIAN_POINT('Ctrl Pts',(89.5750868183844,3.27571919332025,-2.9868298857674));
#19272=CARTESIAN_POINT('Ctrl Pts',(89.5693897252624,3.18995726311767,-3.08088679947362));
#19273=CARTESIAN_POINT('Ctrl Pts',(89.5636926321405,3.10012632529044,-3.17126320461502));
#19274=CARTESIAN_POINT('Ctrl Pts',(89.5579955390185,3.00658179542174,-3.25759956216822));
#19275=CARTESIAN_POINT('Ctrl Pts',(89.552298017245,2.91303022722462,-3.34394241570404));
#19276=CARTESIAN_POINT('Ctrl Pts',(89.5466004954715,2.81576480388216,-3.42624434684018));
#19277=CARTESIAN_POINT('Ctrl Pts',(89.5409029736979,2.71517601201483,-3.50418438781112));
#19278=CARTESIAN_POINT('Ctrl Pts',(89.5352037471007,2.61455712177031,-3.58214775015523));
#19279=CARTESIAN_POINT('Ctrl Pts',(89.5295045205034,2.51061319931515,-3.65574638185656));
#19280=CARTESIAN_POINT('Ctrl Pts',(89.5238052939061,2.40376542905842,-3.72470143260686));
#19281=CARTESIAN_POINT('Ctrl Pts',(89.5180999358819,2.29680270823956,-3.79373066760851));
#19282=CARTESIAN_POINT('Ctrl Pts',(89.5123945778576,2.18693023700328,-3.85810613093712));
#19283=CARTESIAN_POINT('Ctrl Pts',(89.5066892198334,2.07459590672393,-3.91759375430944));
#19284=CARTESIAN_POINT('Ctrl Pts',(89.5009803567025,1.9621925634564,-3.97711792411096));
#19285=CARTESIAN_POINT('Ctrl Pts',(89.4952714935716,1.84732470715158,-4.03174810093616));
#19286=CARTESIAN_POINT('Ctrl Pts',(89.4895626304407,1.73046099961773,-4.08129804459341));
#19287=CARTESIAN_POINT('Ctrl Pts',(89.4838455696813,1.61342948191837,-4.13091913937552));
#19288=CARTESIAN_POINT('Ctrl Pts',(89.4781285089219,1.49439676257133,-4.1754452954221));
#19289=CARTESIAN_POINT('Ctrl Pts',(89.4724114481624,1.37384783026206,-4.21473974751517));
#19290=CARTESIAN_POINT('Ctrl Pts',(89.4699697068177,1.32236170400487,-4.2315223028055));
#19291=CARTESIAN_POINT('Ctrl Pts',(89.467527965473,1.27059914564415,-4.24735116518983));
#19292=CARTESIAN_POINT('Ctrl Pts',(89.4650862241283,1.21859846425015,-4.26221852829336));
#19293=CARTESIAN_POINT('Ctrl Pts',(89.4593811640326,1.09710033218465,-4.29695570475708));
#19294=CARTESIAN_POINT('Ctrl Pts',(89.4536761039369,0.973923986759625,-4.32654844324356));
#19295=CARTESIAN_POINT('Ctrl Pts',(89.4479710438412,0.849543409472067,-4.35083497680877));
#19296=CARTESIAN_POINT('Ctrl Pts',(89.4422730385761,0.725316640187737,-4.37509147784548));
#19297=CARTESIAN_POINT('Ctrl Pts',(89.436575033311,0.599888990771536,-4.39405475140693));
#19298=CARTESIAN_POINT('Ctrl Pts',(89.4308770280459,0.473749623979258,-4.40761276586085));
#19299=CARTESIAN_POINT('Ctrl Pts',(89.4251846424056,0.347734661408601,-4.42115740880135));
#19300=CARTESIAN_POINT('Ctrl Pts',(89.4194922567652,0.221009773679086,-4.4293073572606));
#19301=CARTESIAN_POINT('Ctrl Pts',(89.4137998711249,0.0940738621422794,
-4.43200170447413));
#19302=CARTESIAN_POINT('Ctrl Pts',(89.4081116750029,-0.0327686262916659,
-4.4346940686848));
#19303=CARTESIAN_POINT('Ctrl Pts',(89.4024234788809,-0.159821430762957,
-4.43193881430123));
#19304=CARTESIAN_POINT('Ctrl Pts',(89.3967352827589,-0.286581474138729,
-4.42372694214736));
#19305=CARTESIAN_POINT('Ctrl Pts',(89.3910493038997,-0.413292106360815,
-4.41551827098702));
#19306=CARTESIAN_POINT('Ctrl Pts',(89.3853633250406,-0.539709805735858,
-4.40185723716461));
#19307=CARTESIAN_POINT('Ctrl Pts',(89.3796773461814,-0.665332790061885,
-4.38278693053501));
#19308=CARTESIAN_POINT('Ctrl Pts',(89.3739923495585,-0.790934073384423,
-4.36371991824515));
#19309=CARTESIAN_POINT('Ctrl Pts',(89.3683073529356,-0.915740519226585,
-4.3392455517671));
#19310=CARTESIAN_POINT('Ctrl Pts',(89.3626223563126,-1.03925729366832,-4.3094585828799));
#19311=CARTESIAN_POINT('Ctrl Pts',(89.3569370530937,-1.1627807294588,-4.27967000755997));
#19312=CARTESIAN_POINT('Ctrl Pts',(89.3512517498748,-1.28501396649285,-4.24456835387764));
#19313=CARTESIAN_POINT('Ctrl Pts',(89.3455664466559,-1.40547467608751,-4.20429898257447));
#19314=CARTESIAN_POINT('Ctrl Pts',(89.3398795480991,-1.52596918784376,-4.16401831138937));
#19315=CARTESIAN_POINT('Ctrl Pts',(89.3341926495423,-1.64468980337015,-4.11856716485411));
#19316=CARTESIAN_POINT('Ctrl Pts',(89.3285057509855,-1.76117210416068,-4.06813984758713));
#19317=CARTESIAN_POINT('Ctrl Pts',(89.3228128202523,-1.87777795942903,-4.01765904132816));
#19318=CARTESIAN_POINT('Ctrl Pts',(89.3171198895191,-1.99214039204563,-3.96219168483694));
#19319=CARTESIAN_POINT('Ctrl Pts',(89.3114269587859,-2.10381735312241,-3.90197918301738));
#19320=CARTESIAN_POINT('Ctrl Pts',(89.3057305967038,-2.21556162621179,-3.84173038880016));
#19321=CARTESIAN_POINT('Ctrl Pts',(89.3000342346216,-2.32461686023455,-3.77673095648576));
#19322=CARTESIAN_POINT('Ctrl Pts',(89.2943378725395,-2.43056922637755,-3.70726614040406));
#19323=CARTESIAN_POINT('Ctrl Pts',(89.2886333177804,-2.5366739763561,-3.63770141796354));
#19324=CARTESIAN_POINT('Ctrl Pts',(89.2829287630214,-2.63966662351286,-3.56365872123782));
#19325=CARTESIAN_POINT('Ctrl Pts',(89.2772242082623,-2.73916540771085,-3.48546436923407));
#19326=CARTESIAN_POINT('Ctrl Pts',(89.2746505931735,-2.7840543750618,-3.45018691592227));
#19327=CARTESIAN_POINT('Ctrl Pts',(89.2720769780847,-2.82823269625743,-3.41406495996122));
#19328=CARTESIAN_POINT('Ctrl Pts',(89.2695033629959,-2.87166780824715,-3.37713088272827));
#19329=CARTESIAN_POINT('Ctrl Pts',(89.263865417757,-2.96681987038164,-3.29622045218576));
#19330=CARTESIAN_POINT('Ctrl Pts',(89.2582274725182,-3.05871486481643,-3.21114480803611));
#19331=CARTESIAN_POINT('Ctrl Pts',(89.2525895272793,-3.14696053079779,-3.1221992917815));
#19332=CARTESIAN_POINT('Ctrl Pts',(89.24695849197,-3.23509804189223,-3.03336278815822));
#19333=CARTESIAN_POINT('Ctrl Pts',(89.2413274566606,-3.31959483180976,-2.94066613254748));
#19334=CARTESIAN_POINT('Ctrl Pts',(89.2356964213513,-3.40009127339568,-2.8444451713082));
#19335=CARTESIAN_POINT('Ctrl Pts',(89.2299254421024,-3.48258823327582,-2.7458329019632));
#19336=CARTESIAN_POINT('Ctrl Pts',(89.2241544628535,-3.56088304498919,-2.64351910899112));
#19337=CARTESIAN_POINT('Ctrl Pts',(89.2183834836047,-3.63462789400479,-2.53790643486365));
#19338=CARTESIAN_POINT('Ctrl Pts',(89.2127618304416,-3.70646456952343,-2.43502652523977));
#19339=CARTESIAN_POINT('Ctrl Pts',(89.2071401772786,-3.77398360099277,-2.32901671612977));
#19340=CARTESIAN_POINT('Ctrl Pts',(89.2015185241156,-3.8369041825518,-2.22028270585448));
#19341=CARTESIAN_POINT('Ctrl Pts',(89.1958988209634,-3.89980293853472,-2.11158641268794));
#19342=CARTESIAN_POINT('Ctrl Pts',(89.1902791178113,-3.95810621063216,-2.00016815211306));
#19343=CARTESIAN_POINT('Ctrl Pts',(89.1846594146592,-4.01157734340261,-1.88646129509695));
#19344=CARTESIAN_POINT('Ctrl Pts',(89.1790403124819,-4.06504275793361,-1.77276659796978));
#19345=CARTESIAN_POINT('Ctrl Pts',(89.1734212103047,-4.11367688690895,-1.6567841630041));
#19346=CARTESIAN_POINT('Ctrl Pts',(89.1678021081274,-4.15729003725138,-1.5389699627252));
#19347=CARTESIAN_POINT('Ctrl Pts',(89.161918009065,-4.20295998396949,-1.41559964420594));
#19348=CARTESIAN_POINT('Ctrl Pts',(89.1560339100026,-4.24312361768197,-1.29022102191266));
#19349=CARTESIAN_POINT('Ctrl Pts',(89.1501498109402,-4.27762101250791,-1.16337761425551));
#19350=CARTESIAN_POINT('Ctrl Pts',(89.1445252559786,-4.31059674781946,-1.04212919367123));
#19351=CARTESIAN_POINT('Ctrl Pts',(89.1389007010171,-4.33839540505862,-0.919542878203412));
#19352=CARTESIAN_POINT('Ctrl Pts',(89.1332761460555,-4.36092954124719,-0.796104601341791));
#19353=CARTESIAN_POINT('Ctrl Pts',(89.1276487188446,-4.38347518477421,-0.672603289180431));
#19354=CARTESIAN_POINT('Ctrl Pts',(89.1220212916337,-4.40075089815923,-0.548249555326521));
#19355=CARTESIAN_POINT('Ctrl Pts',(89.1163938644229,-4.41272106872279,-0.42353485057315));
#19356=CARTESIAN_POINT('Ctrl Pts',(89.1107598757896,-4.42470519616957,-0.298674731971114));
#19357=CARTESIAN_POINT('Ctrl Pts',(89.1051258871564,-4.43137141745617,-0.173453211240283));
#19358=CARTESIAN_POINT('Ctrl Pts',(89.0994918985232,-4.43273618773755,-0.048362071109586));
#19359=CARTESIAN_POINT('Ctrl Pts',(89.0987255721416,-4.43292182167107,-0.0313473685561952));
#19360=CARTESIAN_POINT('Ctrl Pts',(89.0979592457601,-4.43300945188702,-0.0143350705708257));
#19361=CARTESIAN_POINT('Ctrl Pts',(89.0971929193785,-4.4329991937622,0.00267359376999083));
#19362=CARTESIAN_POINT('',(87.8471929193744,-4.43299846679216,-0.00368692533081282));
#19363=CARTESIAN_POINT('Ctrl Pts',(89.0971929193385,-4.43299919376167,0.00267359465718153));
#19364=CARTESIAN_POINT('Ctrl Pts',(89.0894354468469,-4.43289535139194,0.174851205810205));
#19365=CARTESIAN_POINT('Ctrl Pts',(89.0816779743552,-4.42276034109812,0.34671858518774));
#19366=CARTESIAN_POINT('Ctrl Pts',(89.0739205018635,-4.40270237763495,0.517398080753629));
#19367=CARTESIAN_POINT('Ctrl Pts',(89.0682090089903,-4.38793456305444,0.643062041994788));
#19368=CARTESIAN_POINT('Ctrl Pts',(89.0624975161171,-4.36775959624138,0.76828670624058));
#19369=CARTESIAN_POINT('Ctrl Pts',(89.0567860232439,-4.34221203575391,0.892571362163206));
#19370=CARTESIAN_POINT('Ctrl Pts',(89.0510814865924,-4.31669559051027,1.01670464757139));
#19371=CARTESIAN_POINT('Ctrl Pts',(89.0453769499408,-4.28581964941365,1.13989981476734));
#19372=CARTESIAN_POINT('Ctrl Pts',(89.0396724132893,-4.24967050494999,1.26166144403248));
#19373=CARTESIAN_POINT('Ctrl Pts',(89.0339734060043,-4.21355639959348,1.38330505062134));
#19374=CARTESIAN_POINT('Ctrl Pts',(89.0282743987194,-4.17217937456742,1.50351750378311));
#19375=CARTESIAN_POINT('Ctrl Pts',(89.0225753914344,-4.12567662877393,1.62181421710028));
#19376=CARTESIAN_POINT('Ctrl Pts',(89.0168804916338,-4.07920739922103,1.74002566962182));
#19377=CARTESIAN_POINT('Ctrl Pts',(89.0111855918331,-4.02761994720952,1.85632376023667));
#19378=CARTESIAN_POINT('Ctrl Pts',(89.0054906920325,-3.97110094773782,1.97024015360459));
#19379=CARTESIAN_POINT('Ctrl Pts',(88.9997979116885,-3.91460298280093,2.08411415099301));
#19380=CARTESIAN_POINT('Ctrl Pts',(88.9941051313445,-3.85317729676634,2.19560785661257));
#19381=CARTESIAN_POINT('Ctrl Pts',(88.9884123510005,-3.78705809782464,2.30427428135212));
#19382=CARTESIAN_POINT('Ctrl Pts',(88.9827204938992,-3.72094962195105,2.41292308280687));
#19383=CARTESIAN_POINT('Ctrl Pts',(88.977028636798,-3.65014935461175,2.51874517459598));
#19384=CARTESIAN_POINT('Ctrl Pts',(88.9713367796967,-3.57493645903895,2.62131995640251));
#19385=CARTESIAN_POINT('Ctrl Pts',(88.9656445641558,-3.49971882699983,2.72390119776622));
#19386=CARTESIAN_POINT('Ctrl Pts',(88.9599523486148,-3.42008825004789,2.82323440055596));
#19387=CARTESIAN_POINT('Ctrl Pts',(88.9542601330738,-3.33636573433397,2.9189300585595));
#19388=CARTESIAN_POINT('Ctrl Pts',(88.9485662774683,-3.25261909614423,3.01465328878989));
#19389=CARTESIAN_POINT('Ctrl Pts',(88.9428724218627,-3.16477843645335,3.10673658900602));
#19390=CARTESIAN_POINT('Ctrl Pts',(88.9371785662572,-3.07320298910899,3.19482587752941));
#19391=CARTESIAN_POINT('Ctrl Pts',(88.931478648168,-2.98153003759703,3.28300895836287));
#19392=CARTESIAN_POINT('Ctrl Pts',(88.9257787300788,-2.88611464662167,3.36718925980919));
#19393=CARTESIAN_POINT('Ctrl Pts',(88.9200788119897,-2.7873508641998,3.44705151685388));
#19394=CARTESIAN_POINT('Ctrl Pts',(88.9143754356075,-2.68852715914599,3.52696222846882));
#19395=CARTESIAN_POINT('Ctrl Pts',(88.9086720592254,-2.58635133585645,3.60254943961233));
#19396=CARTESIAN_POINT('Ctrl Pts',(88.9029686828432,-2.48124701120323,3.67354083540595));
#19397=CARTESIAN_POINT('Ctrl Pts',(88.897257133184,-2.37599206581049,3.74463396608602));
#19398=CARTESIAN_POINT('Ctrl Pts',(88.8915455835248,-2.26780057847517,3.81111792209363));
#19399=CARTESIAN_POINT('Ctrl Pts',(88.8858340338655,-2.15712168492817,3.87276581223454));
#19400=CARTESIAN_POINT('Ctrl Pts',(88.8833352361541,-2.10869977101671,3.89973670734887));
#19401=CARTESIAN_POINT('Ctrl Pts',(88.8808364384426,-2.05980202699204,3.92578256936849));
#19402=CARTESIAN_POINT('Ctrl Pts',(88.8783376407312,-2.01046721161541,3.95088731692253));
#19403=CARTESIAN_POINT('Ctrl Pts',(88.8726271506174,-1.89772260080482,4.00825907297089));
#19404=CARTESIAN_POINT('Ctrl Pts',(88.8669166605037,-1.78234588133867,4.06088971102955));
#19405=CARTESIAN_POINT('Ctrl Pts',(88.86120617039,-1.66477265814443,4.1085302720918));
#19406=CARTESIAN_POINT('Ctrl Pts',(88.8555026574601,-1.54734308811755,4.15611262502378));
#19407=CARTESIAN_POINT('Ctrl Pts',(88.8497991445302,-1.42772272042424,4.19871688203682));
#19408=CARTESIAN_POINT('Ctrl Pts',(88.8440956316003,-1.30637146279836,4.2361400592032));
#19409=CARTESIAN_POINT('Ctrl Pts',(88.8383976676482,-1.18513826845135,4.27352682716304));
#19410=CARTESIAN_POINT('Ctrl Pts',(88.8326997036961,-1.06217791443523,4.30574242848771));
#19411=CARTESIAN_POINT('Ctrl Pts',(88.827001739744,-0.937969539779162,4.33263224177248));
#19412=CARTESIAN_POINT('Ctrl Pts',(88.8213079015606,-0.813851101637493,
4.35950258474307));
#19413=CARTESIAN_POINT('Ctrl Pts',(88.8156140633771,-0.68848683030407,4.38105473060733));
#19414=CARTESIAN_POINT('Ctrl Pts',(88.8099202251937,-0.562369793009557,
4.39718423720344));
#19415=CARTESIAN_POINT('Ctrl Pts',(88.8042285298373,-0.436300218778932,
4.41330767359826));
#19416=CARTESIAN_POINT('Ctrl Pts',(88.798536834481,-0.309478837278903,4.42401247789389));
#19417=CARTESIAN_POINT('Ctrl Pts',(88.7928451391247,-0.182407323016303,
4.42924559812504));
#19418=CARTESIAN_POINT('Ctrl Pts',(88.7871543812534,-0.0553567388350208,
4.43447785640351));
#19419=CARTESIAN_POINT('Ctrl Pts',(88.7814636233821,0.0719434973714359,
4.43424020684309));
#19420=CARTESIAN_POINT('Ctrl Pts',(88.7757728655108,0.198988729714833,4.42853163988319));
#19421=CARTESIAN_POINT('Ctrl Pts',(88.7700817623004,0.326041671696574,4.42282272650346));
#19422=CARTESIAN_POINT('Ctrl Pts',(88.7643906590901,0.452839180153901,4.41164225334748));
#19423=CARTESIAN_POINT('Ctrl Pts',(88.7586995558797,0.578879261437488,4.39504127405848));
#19424=CARTESIAN_POINT('Ctrl Pts',(88.7530068245723,0.704955399961066,4.37843554560169));
#19425=CARTESIAN_POINT('Ctrl Pts',(88.747314093265,0.830273284559471,4.35640627830354));
#19426=CARTESIAN_POINT('Ctrl Pts',(88.7416213619577,0.954339194576103,4.32905598273987));
#19427=CARTESIAN_POINT('Ctrl Pts',(88.7359225802343,1.07853696578984,4.30167661841175));
#19428=CARTESIAN_POINT('Ctrl Pts',(88.730223798511,1.20147971540065,4.26896502030362));
#19429=CARTESIAN_POINT('Ctrl Pts',(88.7245250167877,1.32268671422558,4.23107419646727));
#19430=CARTESIAN_POINT('Ctrl Pts',(88.7188227852243,1.44396708746282,4.19316043487189));
#19431=CARTESIAN_POINT('Ctrl Pts',(88.7131205536609,1.56350924169432,4.15006133685358));
#19432=CARTESIAN_POINT('Ctrl Pts',(88.7074183220975,1.68085178923926,4.10197833521963));
#19433=CARTESIAN_POINT('Ctrl Pts',(88.7017079203398,1.79836246594738,4.05382643994908));
#19434=CARTESIAN_POINT('Ctrl Pts',(88.695997518582,1.91366688115736,4.00067654901692));
#19435=CARTESIAN_POINT('Ctrl Pts',(88.6902871168243,2.02632729424893,3.94277652125781));
#19436=CARTESIAN_POINT('Ctrl Pts',(88.6877763377491,2.07586240925397,3.91731873661866));
#19437=CARTESIAN_POINT('Ctrl Pts',(88.6852655586739,2.12488674171948,3.89094321429857));
#19438=CARTESIAN_POINT('Ctrl Pts',(88.6827547795987,2.17336490489364,3.86367363919064));
#19439=CARTESIAN_POINT('Ctrl Pts',(88.6770433142055,2.28364197149242,3.80164140543018));
#19440=CARTESIAN_POINT('Ctrl Pts',(88.6713318488124,2.3914310796582,3.73478852734399));
#19441=CARTESIAN_POINT('Ctrl Pts',(88.6656203834193,2.49628345568051,3.66333972065051));
#19442=CARTESIAN_POINT('Ctrl Pts',(88.6599158814639,2.60100799533493,3.59197802458137));
#19443=CARTESIAN_POINT('Ctrl Pts',(88.6542113795085,2.7028025991565,3.5160317705608));
#19444=CARTESIAN_POINT('Ctrl Pts',(88.6485068775531,2.80124329905826,3.43577138056088));
#19445=CARTESIAN_POINT('Ctrl Pts',(88.6428079121074,2.89958845724684,3.35558888735738));
#19446=CARTESIAN_POINT('Ctrl Pts',(88.6371089466617,2.9945858811983,3.27110084068346));
#19447=CARTESIAN_POINT('Ctrl Pts',(88.631409981216,3.08584120419349,3.18262047101154));
#19448=CARTESIAN_POINT('Ctrl Pts',(88.6257151303313,3.17703064231818,3.09420398273859));
#19449=CARTESIAN_POINT('Ctrl Pts',(88.6200202794467,3.26448307121504,3.00180118519211));
#19450=CARTESIAN_POINT('Ctrl Pts',(88.6143254285621,3.34783817477462,2.90576471097055));
#19451=CARTESIAN_POINT('Ctrl Pts',(88.6086327075492,3.43116210356169,2.80976415434861));
#19452=CARTESIAN_POINT('Ctrl Pts',(88.6029399865364,3.51039149274652,2.7101329241084));
#19453=CARTESIAN_POINT('Ctrl Pts',(88.5972472655235,3.58520403149405,2.6072592990646));
#19454=CARTESIAN_POINT('Ctrl Pts',(88.5915554742348,3.660004352003,2.50440247514151));
#19455=CARTESIAN_POINT('Ctrl Pts',(88.5858636829461,3.73038902225902,2.39830463238631));
#19456=CARTESIAN_POINT('Ctrl Pts',(88.5801718916574,3.79607739688818,2.28938537534306));
#19457=CARTESIAN_POINT('Ctrl Pts',(88.5744797483686,3.86176983391376,2.18045938235599));
#19458=CARTESIAN_POINT('Ctrl Pts',(88.5687876050798,3.9227651915419,2.06871196982378));
#19459=CARTESIAN_POINT('Ctrl Pts',(88.563095461791,3.97882763391271,1.95458938388926));
#19460=CARTESIAN_POINT('Ctrl Pts',(88.55740168484,4.03490616637246,1.84043404443062));
#19461=CARTESIAN_POINT('Ctrl Pts',(88.5517079078891,4.0860487912224,1.72390253354171));
#19462=CARTESIAN_POINT('Ctrl Pts',(88.5460141309381,4.13206708644723,1.60546273488346));
#19463=CARTESIAN_POINT('Ctrl Pts',(88.5403143008061,4.17813430474638,1.486897020238));
#19464=CARTESIAN_POINT('Ctrl Pts',(88.5346144706741,4.2190661716257,1.36641933955194));
#19465=CARTESIAN_POINT('Ctrl Pts',(88.528914640542,4.25472349518734,1.24451475664246));
#19466=CARTESIAN_POINT('Ctrl Pts',(88.5232113575629,4.29040241926731,1.12253632628974));
#19467=CARTESIAN_POINT('Ctrl Pts',(88.5175080745838,4.32080033946052,0.999129658631843));
#19468=CARTESIAN_POINT('Ctrl Pts',(88.5118047916047,4.34582908841368,0.874790565962802));
#19469=CARTESIAN_POINT('Ctrl Pts',(88.5060933429315,4.37089367236019,0.750273450390316));
#19470=CARTESIAN_POINT('Ctrl Pts',(88.5003818942583,4.39057367356081,0.62482163752853));
#19471=CARTESIAN_POINT('Ctrl Pts',(88.4946704455851,4.40483267249706,0.498936997327742));
#19472=CARTESIAN_POINT('Ctrl Pts',(88.4921709365455,4.41107285756669,0.443845931272622));
#19473=CARTESIAN_POINT('Ctrl Pts',(88.489671427506,4.41627547989079,0.388671984248708));
#19474=CARTESIAN_POINT('Ctrl Pts',(88.4871719184664,4.42044062562448,0.333457156661257));
#19475=CARTESIAN_POINT('Ctrl Pts',(88.4814607422868,4.42995764705641,0.207295737323731));
#19476=CARTESIAN_POINT('Ctrl Pts',(88.4757495661071,4.43408399449798,0.0805319756985775));
#19477=CARTESIAN_POINT('Ctrl Pts',(88.4700383899275,4.43275782838372,-0.0463361079808987));
#19478=CARTESIAN_POINT('Ctrl Pts',(88.4643341796299,4.43143327978509,-0.173049451537361));
#19479=CARTESIAN_POINT('Ctrl Pts',(88.4586299693323,4.42466945260335,-0.299866468287363));
#19480=CARTESIAN_POINT('Ctrl Pts',(88.4529257590347,4.4124562977987,-0.426284435578654));
#19481=CARTESIAN_POINT('Ctrl Pts',(88.4472270873202,4.40025500152826,-0.552579655568815));
#19482=CARTESIAN_POINT('Ctrl Pts',(88.4415284156057,4.38261494433749,-0.678476202027556));
#19483=CARTESIAN_POINT('Ctrl Pts',(88.4358297438912,4.3595781156314,-0.803472248249908));
#19484=CARTESIAN_POINT('Ctrl Pts',(88.4301351884441,4.3365579268985,-0.928378007268043));
#19485=CARTESIAN_POINT('Ctrl Pts',(88.4244406329968,4.30814879734629,-1.05238416943556));
#19486=CARTESIAN_POINT('Ctrl Pts',(88.4187460775497,4.27444438719986,-1.1749953960487));
#19487=CARTESIAN_POINT('Ctrl Pts',(88.41305365341,4.24075259164037,-1.29756073282213));
#19488=CARTESIAN_POINT('Ctrl Pts',(88.4073612292704,4.20176956173012,-1.41873178786164));
#19489=CARTESIAN_POINT('Ctrl Pts',(88.4016688051308,4.15763969562153,-1.53802508477336));
#19490=CARTESIAN_POINT('Ctrl Pts',(88.3959773115169,4.11351704330688,-1.65729888112146));
#19491=CARTESIAN_POINT('Ctrl Pts',(88.390285817903,4.06424936672886,-1.77469515566863));
#19492=CARTESIAN_POINT('Ctrl Pts',(88.3845943242891,4.01003023584544,-1.88974773649959));
#19493=CARTESIAN_POINT('Ctrl Pts',(88.3789024791523,3.95580775623424,-2.0048074233053));
#19494=CARTESIAN_POINT('Ctrl Pts',(88.3732106340156,3.89663338424477,-2.11752276741075));
#19495=CARTESIAN_POINT('Ctrl Pts',(88.3675187888788,3.83274770655572,-2.22745011569101));
#19496=CARTESIAN_POINT('Ctrl Pts',(88.361825310233,3.7688436942437,-2.3374090121454));
#19497=CARTESIAN_POINT('Ctrl Pts',(88.3561318315872,3.70022588691505,-2.44457797606595));
#19498=CARTESIAN_POINT('Ctrl Pts',(88.3504383529414,3.62717916722803,-2.54854081560939));
#19499=CARTESIAN_POINT('Ctrl Pts',(88.3447388197215,3.55405476800685,-2.65261421158823));
#19500=CARTESIAN_POINT('Ctrl Pts',(88.3390392865017,3.47649228245226,-2.75347434892433));
#19501=CARTESIAN_POINT('Ctrl Pts',(88.3333397532819,3.39481818658066,-2.85073648029087));
#19502=CARTESIAN_POINT('Ctrl Pts',(88.3276367668201,3.31309460588234,-2.94805754098703));
#19503=CARTESIAN_POINT('Ctrl Pts',(88.3219337803584,3.22725472136438,-3.04177595910031));
#19504=CARTESIAN_POINT('Ctrl Pts',(88.3162307938966,3.13766224411753,-3.13154349192844));
#19505=CARTESIAN_POINT('Ctrl Pts',(88.3105196385554,3.04794143583697,-3.22143960653748));
#19506=CARTESIAN_POINT('Ctrl Pts',(88.3048084832142,2.95445759510588,-3.30737326625973));
#19507=CARTESIAN_POINT('Ctrl Pts',(88.2990973278729,2.8576081652666,-3.38903593574953));
#19508=CARTESIAN_POINT('Ctrl Pts',(88.2965945710266,2.81516656473057,-3.42482235599943));
#19509=CARTESIAN_POINT('Ctrl Pts',(88.2940918141803,2.77207902670282,-3.45978913373035));
#19510=CARTESIAN_POINT('Ctrl Pts',(88.291589057334,2.72838069256191,-3.49391296349171));
#19511=CARTESIAN_POINT('Ctrl Pts',(88.2858779581601,2.62866444550436,-3.57178092587354));
#19512=CARTESIAN_POINT('Ctrl Pts',(88.2801668589862,2.52545816082209,-3.64549679102386));
#19513=CARTESIAN_POINT('Ctrl Pts',(88.2744557598124,2.4191419936789,-3.71473296677154));
#19514=CARTESIAN_POINT('Ctrl Pts',(88.2687516284963,2.31295553815734,-3.78388467054404));
#19515=CARTESIAN_POINT('Ctrl Pts',(88.2630474971802,2.2036670803463,-3.84856734239221));
#19516=CARTESIAN_POINT('Ctrl Pts',(88.2573433658642,2.09168940537722,-3.90849388274214));
#19517=CARTESIAN_POINT('Ctrl Pts',(88.2516447750012,1.97982049491967,-3.96836221612455));
#19518=CARTESIAN_POINT('Ctrl Pts',(88.2459461841382,1.86526791486414,-4.02348342317211));
#19519=CARTESIAN_POINT('Ctrl Pts',(88.2402475932753,1.74847255868385,-4.073614207498));
#19520=CARTESIAN_POINT('Ctrl Pts',(88.234553120446,1.63176160358075,-4.12370876527913));
#19521=CARTESIAN_POINT('Ctrl Pts',(88.2288586476166,1.51281146363334,-4.16881992102407));
#19522=CARTESIAN_POINT('Ctrl Pts',(88.2231641747873,1.3920862829569,-4.20875097633529));
#19523=CARTESIAN_POINT('Ctrl Pts',(88.2174718355986,1.27140633634445,-4.24866707002954));
#19524=CARTESIAN_POINT('Ctrl Pts',(88.2117794964099,1.14895304977384,-4.28340679732801));
#19525=CARTESIAN_POINT('Ctrl Pts',(88.2060871572212,1.02520882789455,-4.31282226149039));
#19526=CARTESIAN_POINT('Ctrl Pts',(88.2003957499874,0.901484865528564,-4.342232909727));
#19527=CARTESIAN_POINT('Ctrl Pts',(88.1947043427534,0.776470776461303,-4.36632093641831));
#19528=CARTESIAN_POINT('Ctrl Pts',(88.1890129355195,0.650661828547268,-4.3849889606328));
#19529=CARTESIAN_POINT('Ctrl Pts',(88.1833211781036,0.52484513983484,-4.40365813345726));
#19530=CARTESIAN_POINT('Ctrl Pts',(88.1776294206876,0.398233889867758,-4.41690658195273));
#19531=CARTESIAN_POINT('Ctrl Pts',(88.1719376632717,0.271330675230027,-4.4246885387199));
#19532=CARTESIAN_POINT('Ctrl Pts',(88.1662442736,0.144391067878774,-4.43247272716043));
#19533=CARTESIAN_POINT('Ctrl Pts',(88.1605508839284,0.0171597275565208,
-4.43478728084396));
#19534=CARTESIAN_POINT('Ctrl Pts',(88.1548574942567,-0.109859042330854,
-4.43163852212905));
#19535=CARTESIAN_POINT('Ctrl Pts',(88.1491580514315,-0.23701285727201,-4.42848641568616));
#19536=CARTESIAN_POINT('Ctrl Pts',(88.1434586086063,-0.363953251139066,
-4.41985940935115));
#19537=CARTESIAN_POINT('Ctrl Pts',(88.1377591657811,-0.490179027338487,
-4.40581587463179));
#19538=CARTESIAN_POINT('Ctrl Pts',(88.13205627065,-0.616481261888762,-4.39176383336538));
#19539=CARTESIAN_POINT('Ctrl Pts',(88.1263533755188,-0.742067622648898,
-4.37228878877165));
#19540=CARTESIAN_POINT('Ctrl Pts',(88.1206504803877,-0.866446647464566,
-4.3475003400917));
#19541=CARTESIAN_POINT('Ctrl Pts',(88.1149394170264,-0.991003819777342,
-4.32267638703232));
#19542=CARTESIAN_POINT('Ctrl Pts',(88.1092283536652,-1.11434981633043,-4.2925239283635));
#19543=CARTESIAN_POINT('Ctrl Pts',(88.1035172903039,-1.23600751705262,-4.25720265171737));
#19544=CARTESIAN_POINT('Ctrl Pts',(88.1010135922699,-1.28934156832493,-4.24171800283394));
#19545=CARTESIAN_POINT('Ctrl Pts',(88.0985098942358,-1.34235139342916,-4.22524059022021));
#19546=CARTESIAN_POINT('Ctrl Pts',(88.0960061962017,-1.39499806833746,-4.2077867566376));
#19547=CARTESIAN_POINT('Ctrl Pts',(88.0902949857889,-1.51509092052739,-4.16797264377605));
#19548=CARTESIAN_POINT('Ctrl Pts',(88.0845837753762,-1.6336631609298,-4.12295174897156));
#19549=CARTESIAN_POINT('Ctrl Pts',(88.0788725649634,-1.75023137394233,-4.07285884087184));
#19550=CARTESIAN_POINT('Ctrl Pts',(88.073168320749,-1.86665740390753,-4.02282703315394));
#19551=CARTESIAN_POINT('Ctrl Pts',(88.0674640765346,-1.98108390597914,-3.96773567640255));
#19552=CARTESIAN_POINT('Ctrl Pts',(88.0617598323203,-2.09304307445528,-3.90776914472628));
#19553=CARTESIAN_POINT('Ctrl Pts',(88.056061127046,-2.20489352824358,-3.84786084180306));
#19554=CARTESIAN_POINT('Ctrl Pts',(88.0503624217718,-2.31428106592543,-3.78308697113222));
#19555=CARTESIAN_POINT('Ctrl Pts',(88.0446637164975,-2.42075875350021,-3.71367958463733));
#19556=CARTESIAN_POINT('Ctrl Pts',(88.0389691278883,-2.5271595230825,-3.64432233706784));
#19557=CARTESIAN_POINT('Ctrl Pts',(88.033274539279,-2.63065429300325,-3.57033845281576));
#19558=CARTESIAN_POINT('Ctrl Pts',(88.0275799506697,-2.73082201984094,-3.49200516837416));
#19559=CARTESIAN_POINT('Ctrl Pts',(88.0218874940895,-2.83095224432101,-3.41370121157071));
#19560=CARTESIAN_POINT('Ctrl Pts',(88.0161950375092,-2.92775758853443,-3.33105133786086));
#19561=CARTESIAN_POINT('Ctrl Pts',(88.010502580929,-3.02084749990109,-3.2443750372516));
#19562=CARTESIAN_POINT('Ctrl Pts',(88.004811055335,-3.11392218665838,-3.1577129123226));
#19563=CARTESIAN_POINT('Ctrl Pts',(87.999119529741,-3.20328235721564,-3.06702594223288));
#19564=CARTESIAN_POINT('Ctrl Pts',(87.993428004147,-3.28857236869048,-2.97267232904763));
#19565=CARTESIAN_POINT('Ctrl Pts',(87.9877361275281,-3.37386764042707,-2.87831289660297));
#19566=CARTESIAN_POINT('Ctrl Pts',(87.9820442509093,-3.45509198614297,-2.78028666741058));
#19567=CARTESIAN_POINT('Ctrl Pts',(87.9763523742904,-3.53192865445068,-2.67898655835938));
#19568=CARTESIAN_POINT('Ctrl Pts',(87.9706588646982,-3.60878736684661,-2.57765738677085));
#19569=CARTESIAN_POINT('Ctrl Pts',(87.964965355106,-3.68125565651211,-2.47305278469922));
#19570=CARTESIAN_POINT('Ctrl Pts',(87.9592718455138,-3.74905917663427,-2.36559596932662));
#19571=CARTESIAN_POINT('Ctrl Pts',(87.9535722823306,-3.8169347884554,-2.25802490111918));
#19572=CARTESIAN_POINT('Ctrl Pts',(87.9478727191474,-3.88013551477021,-2.14759590255314));
#19573=CARTESIAN_POINT('Ctrl Pts',(87.9421731559642,-3.93843204822112,-2.03475846270382));
#19574=CARTESIAN_POINT('Ctrl Pts',(87.9364701400612,-3.99676389693887,-1.92185266742987));
#19575=CARTESIAN_POINT('Ctrl Pts',(87.9307671241582,-4.05018546690914,-1.80653588594852));
#19576=CARTESIAN_POINT('Ctrl Pts',(87.9250641082552,-4.09851548105195,-1.6892779083317));
#19577=CARTESIAN_POINT('Ctrl Pts',(87.9193529245336,-4.14691471309565,-1.57185199467724));
#19578=CARTESIAN_POINT('Ctrl Pts',(87.913641740812,-4.19020769294354,-1.4524797079483));
#19579=CARTESIAN_POINT('Ctrl Pts',(87.9079305570904,-4.22826278018989,-1.33164667298082));
#19580=CARTESIAN_POINT('Ctrl Pts',(87.90542814975,-4.24493696444051,-1.2787025744542));
#19581=CARTESIAN_POINT('Ctrl Pts',(87.9029257424097,-4.26060622023336,-1.22547817995853));
#19582=CARTESIAN_POINT('Ctrl Pts',(87.9004233350693,-4.27526257954052,-1.17201487873684));
#19583=CARTESIAN_POINT('Ctrl Pts',(87.8932731563333,-4.31714048925394,-1.01925311473932));
#19584=CARTESIAN_POINT('Ctrl Pts',(87.8861229775972,-4.35084897738077,-0.864164255937209));
#19585=CARTESIAN_POINT('Ctrl Pts',(87.8789727988612,-4.37617406990347,-0.70752350484245));
#19586=CARTESIAN_POINT('Ctrl Pts',(87.8719271935475,-4.40112877565772,-0.553173669824393));
#19587=CARTESIAN_POINT('Ctrl Pts',(87.8648815882338,-4.41794351585947,-0.397316902218557));
#19588=CARTESIAN_POINT('Ctrl Pts',(87.85783598292,-4.42645967010616,-0.240715161391253));
#19589=CARTESIAN_POINT('Ctrl Pts',(87.8542882950715,-4.43074782642376,-0.161861171101559));
#19590=CARTESIAN_POINT('Ctrl Pts',(87.850740607223,-4.43293265294547,-0.0828186286532786));
#19591=CARTESIAN_POINT('Ctrl Pts',(87.8471929193744,-4.43299846679216,-0.00368692533081282));
#19592=CARTESIAN_POINT('',(86.5971929193007,-4.43299889626788,0.00312820839395853));
#19593=CARTESIAN_POINT('Ctrl Pts',(87.8471929193385,-4.43299846679282,-0.00368692453002637));
#19594=CARTESIAN_POINT('Ctrl Pts',(87.8412615674468,-4.43310850043048,0.128612758598833));
#19595=CARTESIAN_POINT('Ctrl Pts',(87.8353302155551,-4.42729075618896,0.261038035339765));
#19596=CARTESIAN_POINT('Ctrl Pts',(87.8293988636633,-4.41554413589774,0.393012702007276));
#19597=CARTESIAN_POINT('Ctrl Pts',(87.8237577098415,-4.40437223223067,0.518530359507987));
#19598=CARTESIAN_POINT('Ctrl Pts',(87.8181165560196,-4.38783787641083,0.64363999588161));
#19599=CARTESIAN_POINT('Ctrl Pts',(87.8124754021977,-4.36599350192544,0.767847472578289));
#19600=CARTESIAN_POINT('Ctrl Pts',(87.8068353578439,-4.34415342365963,0.89203052089888));
#19601=CARTESIAN_POINT('Ctrl Pts',(87.80119531349,-4.3170054737535,1.0153113613675));
#19602=CARTESIAN_POINT('Ctrl Pts',(87.7955552691362,-4.28465359414585,1.13720384196198));
#19603=CARTESIAN_POINT('Ctrl Pts',(87.7899150029168,-4.25230044189391,1.25910111751025));
#19604=CARTESIAN_POINT('Ctrl Pts',(87.7842747366973,-4.2147430577544,1.37960953098333));
#19605=CARTESIAN_POINT('Ctrl Pts',(87.7786344704778,-4.17213570277715,1.49825654599346));
#19606=CARTESIAN_POINT('Ctrl Pts',(87.7729926511568,-4.12951661545433,1.6169362316019));
#19607=CARTESIAN_POINT('Ctrl Pts',(87.7673508318357,-4.0818449301354,1.73375311648484));
#19608=CARTESIAN_POINT('Ctrl Pts',(87.7617090125146,-4.02932340739154,1.84825373762551));
#19609=CARTESIAN_POINT('Ctrl Pts',(87.7560612407086,-3.97674647103854,1.96287516433947));
#19610=CARTESIAN_POINT('Ctrl Pts',(87.7504134689026,-3.91930965343418,2.07517507880274));
#19611=CARTESIAN_POINT('Ctrl Pts',(87.7447656970966,-3.85726220666753,2.184723613873));
#19612=CARTESIAN_POINT('Ctrl Pts',(87.7391144537161,-3.79517662055247,2.29433948627888));
#19613=CARTESIAN_POINT('Ctrl Pts',(87.7334632103356,-3.72847497780001,2.40120026736829));
#19614=CARTESIAN_POINT('Ctrl Pts',(87.7278119669551,-3.65744957676044,2.50490550589337));
#19615=CARTESIAN_POINT('Ctrl Pts',(87.7221526948006,-3.5863232692746,2.60875807941303));
#19616=CARTESIAN_POINT('Ctrl Pts',(87.7164934226462,-3.51086118639162,2.70944583774612));
#19617=CARTESIAN_POINT('Ctrl Pts',(87.7108341504918,-3.43139567019841,2.80660163802125));
#19618=CARTESIAN_POINT('Ctrl Pts',(87.7088362583068,-3.40334196833646,2.84090053879793));
#19619=CARTESIAN_POINT('Ctrl Pts',(87.7068383661219,-3.3747896503618,2.87475959036286));
#19620=CARTESIAN_POINT('Ctrl Pts',(87.7048404739369,-3.34575438665027,2.90816378221903));
#19621=CARTESIAN_POINT('Ctrl Pts',(87.6991293093837,-3.26275432781231,3.00365283708149));
#19622=CARTESIAN_POINT('Ctrl Pts',(87.6934181448304,-3.175535045002,3.09573308792214));
#19623=CARTESIAN_POINT('Ctrl Pts',(87.6877069802772,-3.08440710509131,3.18401033447792));
#19624=CARTESIAN_POINT('Ctrl Pts',(87.6820027825159,-2.99339032804251,3.27217989560401));
#19625=CARTESIAN_POINT('Ctrl Pts',(87.6762985847546,-2.89847466397116,3.35655540652586));
#19626=CARTESIAN_POINT('Ctrl Pts',(87.6705943869933,-2.80001044521793,3.43677617930969));
#19627=CARTESIAN_POINT('Ctrl Pts',(87.6648957287057,-2.70164184726516,3.51691904791061));
#19628=CARTESIAN_POINT('Ctrl Pts',(87.6591970704182,-2.59973185954931,3.59291495626663));
#19629=CARTESIAN_POINT('Ctrl Pts',(87.6534984121306,-2.49466677417512,3.66444084217861));
#19630=CARTESIAN_POINT('Ctrl Pts',(87.6478038709826,-2.38967759572394,3.73591505240884));
#19631=CARTESIAN_POINT('Ctrl Pts',(87.6421093298346,-2.28153818529909,3.80292544397902));
#19632=CARTESIAN_POINT('Ctrl Pts',(87.6364147886866,-2.17066656065766,3.86519025177838));
#19633=CARTESIAN_POINT('Ctrl Pts',(87.6307223800985,-2.05983645655062,3.9274317419065));
#19634=CARTESIAN_POINT('Ctrl Pts',(87.6250299715105,-1.94627652014265,3.98493098676285));
#19635=CARTESIAN_POINT('Ctrl Pts',(87.6193375629225,-1.83043201790219,4.03745063472465));
#19636=CARTESIAN_POINT('Ctrl Pts',(87.6136460856369,-1.71460646831836,4.08996169024715));
#19637=CARTESIAN_POINT('Ctrl Pts',(87.6079546083513,-1.59649745976387,4.13749460459382));
#19638=CARTESIAN_POINT('Ctrl Pts',(87.6022631310657,-1.47657253710115,4.17985915344987));
#19639=CARTESIAN_POINT('Ctrl Pts',(87.5965713030196,-1.35664022357751,4.22222631319348));
#19640=CARTESIAN_POINT('Ctrl Pts',(87.5908794749736,-1.23489214974176,4.25942434098187));
#19641=CARTESIAN_POINT('Ctrl Pts',(87.5851876469276,-1.1118129162237,4.29131227473813));
#19642=CARTESIAN_POINT('Ctrl Pts',(87.5794941861211,-0.988698376139835,
4.32320935588181));
#19643=CARTESIAN_POINT('Ctrl Pts',(87.5738007253147,-0.864252302975927,
4.34979321263873));
#19644=CARTESIAN_POINT('Ctrl Pts',(87.5681072645082,-0.738970925940442,
4.37097368679048));
#19645=CARTESIAN_POINT('Ctrl Pts',(87.5624077501686,-0.613556344340249,
4.39217668093606));
#19646=CARTESIAN_POINT('Ctrl Pts',(87.556708235829,-0.487305079536574,4.40796475512485));
#19647=CARTESIAN_POINT('Ctrl Pts',(87.5510087214894,-0.360720256752866,
4.41829943489213));
#19648=CARTESIAN_POINT('Ctrl Pts',(87.5453057545294,-0.234058752112526,
4.42864037514479));
#19649=CARTESIAN_POINT('Ctrl Pts',(87.5396027875694,-0.107063685173065,
4.43352132465323));
#19650=CARTESIAN_POINT('Ctrl Pts',(87.5338998206094,0.0197615851498626,
4.43295595283242));
#19651=CARTESIAN_POINT('Ctrl Pts',(87.5281886855587,0.146768501327744,4.4323897712562));
#19652=CARTESIAN_POINT('Ctrl Pts',(87.522477550508,0.273604737472531,4.42636171148116));
#19653=CARTESIAN_POINT('Ctrl Pts',(87.5167664154573,0.399771441374032,4.41493734889429));
#19654=CARTESIAN_POINT('Ctrl Pts',(87.5142634812398,0.455064646229623,4.40993056341661));
#19655=CARTESIAN_POINT('Ctrl Pts',(87.5117605470222,0.510229377559847,4.40388798793471));
#19656=CARTESIAN_POINT('Ctrl Pts',(87.5092576128046,0.565224344161995,4.3968182178442));
#19657=CARTESIAN_POINT('Ctrl Pts',(87.5035464360579,0.690711451347686,4.38068646885081));
#19658=CARTESIAN_POINT('Ctrl Pts',(87.4978352593113,0.815700963541726,4.35915337948087));
#19659=CARTESIAN_POINT('Ctrl Pts',(87.4921240825646,0.939692625398773,4.3322588530432));
#19660=CARTESIAN_POINT('Ctrl Pts',(87.486419872417,1.06353303993185,4.30539713304664));
#19661=CARTESIAN_POINT('Ctrl Pts',(87.4807156622695,1.1863776389725,4.27318707104068));
#19662=CARTESIAN_POINT('Ctrl Pts',(87.4750114521219,1.30773200965324,4.23572024464887));
#19663=CARTESIAN_POINT('Ctrl Pts',(87.4693127812714,1.42896853441169,4.19828980188863));
#19664=CARTESIAN_POINT('Ctrl Pts',(87.4636141104209,1.54871733117747,4.15561286962637));
#19665=CARTESIAN_POINT('Ctrl Pts',(87.4579154395704,1.66649536283774,4.10783181321245));
#19666=CARTESIAN_POINT('Ctrl Pts',(87.4522208856985,1.78418830629793,4.06008527600412));
#19667=CARTESIAN_POINT('Ctrl Pts',(87.4465263318267,1.89991294977084,4.00724210333145));
#19668=CARTESIAN_POINT('Ctrl Pts',(87.4408317779548,2.01320303481319,3.94949396006868));
#19669=CARTESIAN_POINT('Ctrl Pts',(87.4351393564502,2.12645069755636,3.89176744101962));
#19670=CARTESIAN_POINT('Ctrl Pts',(87.4294469349457,2.23726525946651,3.82913978433716));
#19671=CARTESIAN_POINT('Ctrl Pts',(87.4237545134411,2.34520231646116,3.76184995645297));
#19672=CARTESIAN_POINT('Ctrl Pts',(87.4180630231227,2.45312171673464,3.6945711360741));
#19673=CARTESIAN_POINT('Ctrl Pts',(87.4123715328043,2.55816420977772,3.62263187257006));
#19674=CARTESIAN_POINT('Ctrl Pts',(87.4066800424859,2.65991226009746,3.54631580215062));
#19675=CARTESIAN_POINT('Ctrl Pts',(87.4009882013048,2.76166658286984,3.46999502708146));
#19676=CARTESIAN_POINT('Ctrl Pts',(87.3952963601237,2.86012573966043,3.38929714797341));
#19677=CARTESIAN_POINT('Ctrl Pts',(87.3896045189425,2.95490373590428,3.30454730811029));
#19678=CARTESIAN_POINT('Ctrl Pts',(87.3839110449123,3.04970892162158,3.21977315560485));
#19679=CARTESIAN_POINT('Ctrl Pts',(87.378217570882,3.14083054854304,3.13094499587316));
#19680=CARTESIAN_POINT('Ctrl Pts',(87.3725240968518,3.22791845502371,3.03842581737934));
#19681=CARTESIAN_POINT('Ctrl Pts',(87.3668245692257,3.31509895786811,2.94580826771265));
#19682=CARTESIAN_POINT('Ctrl Pts',(87.3611250415996,3.39823690325468,2.84949215452158));
#19683=CARTESIAN_POINT('Ctrl Pts',(87.3554255139734,3.47702131862471,2.74987486075808));
#19684=CARTESIAN_POINT('Ctrl Pts',(87.349722533673,3.55585346021824,2.65019722057703));
#19685=CARTESIAN_POINT('Ctrl Pts',(87.3440195533725,3.6303265844766,2.54721473890253));
#19686=CARTESIAN_POINT('Ctrl Pts',(87.3383165730721,3.70017298468677,2.44135390375796));
#19687=CARTESIAN_POINT('Ctrl Pts',(87.3326054247137,3.77011942196735,2.33534145009349));
#19688=CARTESIAN_POINT('Ctrl Pts',(87.3268942763553,3.83542569861879,2.22644275284825));
#19689=CARTESIAN_POINT('Ctrl Pts',(87.3211831279969,3.8958698040357,2.11510932814426));
#19690=CARTESIAN_POINT('Ctrl Pts',(87.3186803358887,3.92235817739518,2.06631976792811));
#19691=CARTESIAN_POINT('Ctrl Pts',(87.3161775437804,3.94791341649992,2.01706289789703));
#19692=CARTESIAN_POINT('Ctrl Pts',(87.3136747516722,3.97251978385321,1.96737784039946));
#19693=CARTESIAN_POINT('Ctrl Pts',(87.3079635806114,4.02866954262647,1.85400052008763));
#19694=CARTESIAN_POINT('Ctrl Pts',(87.3022524095507,4.08004830297613,1.73804259426207));
#19695=CARTESIAN_POINT('Ctrl Pts',(87.2965412384899,4.12641191158218,1.61994251007642));
#19696=CARTESIAN_POINT('Ctrl Pts',(87.2908370340932,4.17271896441743,1.50198648804413));
#19697=CARTESIAN_POINT('Ctrl Pts',(87.2851328296964,4.2140228918231,1.38189387467903));
#19698=CARTESIAN_POINT('Ctrl Pts',(87.2794286252996,4.25012578432657,1.26012690527679));
#19699=CARTESIAN_POINT('Ctrl Pts',(87.2737299602574,4.28619361730083,1.13847818381328));
#19700=CARTESIAN_POINT('Ctrl Pts',(87.2680312952151,4.31707035277037,1.01515872228983));
#19701=CARTESIAN_POINT('Ctrl Pts',(87.2623326301728,4.34260665515484,0.890649447653165));
#19702=CARTESIAN_POINT('Ctrl Pts',(87.2566380821594,4.36812450871079,0.766230125360507));
#19703=CARTESIAN_POINT('Ctrl Pts',(87.2509435341461,4.38830952828994,0.640623090475924));
#19704=CARTESIAN_POINT('Ctrl Pts',(87.2452489861327,4.40306270929082,0.514322640034989));
#19705=CARTESIAN_POINT('Ctrl Pts',(87.2395565705395,4.41781036571238,0.388069484943883));
#19706=CARTESIAN_POINT('Ctrl Pts',(87.2338641549464,4.42713018167997,0.26112382640866));
#19707=CARTESIAN_POINT('Ctrl Pts',(87.2281717393533,4.430974634992,0.133987999677086));
#19708=CARTESIAN_POINT('Ctrl Pts',(87.2224802549776,4.4348184593932,0.00687297098711359));
#19709=CARTESIAN_POINT('Ctrl Pts',(87.2167887706019,4.43318869072357,-0.120431765188496));
#19710=CARTESIAN_POINT('Ctrl Pts',(87.2110972862262,4.42608987904782,-0.247421467521375));
#19711=CARTESIAN_POINT('Ctrl Pts',(87.2054054510125,4.41899062978273,-0.374418997832107));
#19712=CARTESIAN_POINT('Ctrl Pts',(87.1997136157988,4.40642168928279,-0.501101057126508));
#19713=CARTESIAN_POINT('Ctrl Pts',(87.1940217805851,4.38843963833758,-0.626966139968921));
#19714=CARTESIAN_POINT('Ctrl Pts',(87.1883283125408,4.37045242883763,-0.752867330034119));
#19715=CARTESIAN_POINT('Ctrl Pts',(87.1826348444964,4.3470490761229,-0.877950682418883));
#19716=CARTESIAN_POINT('Ctrl Pts',(87.1769413764521,4.31833752384674,-1.00172352979112));
#19717=CARTESIAN_POINT('Ctrl Pts',(87.1712418548072,4.28959544390871,-1.1256279790913));
#19718=CARTESIAN_POINT('Ctrl Pts',(87.1655423331624,4.25553398588382,-1.24821875212503));
#19719=CARTESIAN_POINT('Ctrl Pts',(87.1598428115176,4.21631144533384,-1.36901672595584));
#19720=CARTESIAN_POINT('Ctrl Pts',(87.1541398372039,4.17706514446639,-1.48988787705074));
#19721=CARTESIAN_POINT('Ctrl Pts',(87.1484368628902,4.13265167199479,-1.60896369203366));
#19722=CARTESIAN_POINT('Ctrl Pts',(87.1427338885766,4.08327753372543,-1.72578491781947));
#19723=CARTESIAN_POINT('Ctrl Pts',(87.1370227461614,4.03383267920321,-1.84277346114501));
#19724=CARTESIAN_POINT('Ctrl Pts',(87.1313116037462,3.97941314270378,-1.95750060760015));
#19725=CARTESIAN_POINT('Ctrl Pts',(87.125600461331,3.92027159475806,-2.06953125691136));
#19726=CARTESIAN_POINT('Ctrl Pts',(87.1230976044006,3.89435334191318,-2.11862768397628));
#19727=CARTESIAN_POINT('Ctrl Pts',(87.1205947474702,3.86752876863485,-2.16720660325151));
#19728=CARTESIAN_POINT('Ctrl Pts',(87.1180918905398,3.83982170988911,-2.21523322389863));
#19729=CARTESIAN_POINT('Ctrl Pts',(87.1123807193201,3.77659805752225,-2.32482328887132));
#19730=CARTESIAN_POINT('Ctrl Pts',(87.1066695481004,3.70858153221895,-2.43187360557027));
#19731=CARTESIAN_POINT('Ctrl Pts',(87.1009583768807,3.63600165180871,-2.53593789120403));
#19732=CARTESIAN_POINT('Ctrl Pts',(87.095254172336,3.56351030673041,-2.63987523578994));
#19733=CARTESIAN_POINT('Ctrl Pts',(87.0895499677914,3.48646690744268,-2.74083347132593));
#19734=CARTESIAN_POINT('Ctrl Pts',(87.0838457632467,3.40514640826533,-2.83839161115547));
#19735=CARTESIAN_POINT('Ctrl Pts',(87.0781470980677,3.32390487960515,-2.93585501205897));
#19736=CARTESIAN_POINT('Ctrl Pts',(87.0724484328887,3.23839477006315,-3.02992458256673));
#19737=CARTESIAN_POINT('Ctrl Pts',(87.0667497677097,3.14893352089849,-3.12020939697352));
#19738=CARTESIAN_POINT('Ctrl Pts',(87.061055219571,3.05953690363478,-3.21042898448892));
#19739=CARTESIAN_POINT('Ctrl Pts',(87.0553606714323,2.96619510811612,-3.29686897546491));
#19740=CARTESIAN_POINT('Ctrl Pts',(87.0496661232935,2.86926460800952,-3.37917291792296));
#19741=CARTESIAN_POINT('Ctrl Pts',(87.0439737075925,2.77237040547232,-3.46144604001941));
#19742=CARTESIAN_POINT('Ctrl Pts',(87.0382812918915,2.67189047416994,-3.53958593524632));
#19743=CARTESIAN_POINT('Ctrl Pts',(87.0325888761905,2.5682165212555,-3.6132745397977));
#19744=CARTESIAN_POINT('Ctrl Pts',(87.0268973917179,2.46455952847356,-3.6869510895517));
#19745=CARTESIAN_POINT('Ctrl Pts',(87.0212059072452,2.35770987863441,-3.75617756590147));
#19746=CARTESIAN_POINT('Ctrl Pts',(87.0155144227726,2.24809015223047,-3.82067790679146));
#19747=CARTESIAN_POINT('Ctrl Pts',(87.009822587473,2.13846366879342,-3.88518222352552));
#19748=CARTESIAN_POINT('Ctrl Pts',(87.0041307521735,2.02606711322478,-3.94495962296032));
#19749=CARTESIAN_POINT('Ctrl Pts',(86.9984389168739,1.91134922094013,-3.99977913835396));
#19750=CARTESIAN_POINT('Ctrl Pts',(86.992745448755,1.79659841948137,-4.054614379847));
#19751=CARTESIAN_POINT('Ctrl Pts',(86.987051980636,1.67952531656237,-4.10448873587591));
#19752=CARTESIAN_POINT('Ctrl Pts',(86.9813585125171,1.56059976994032,-4.14921888529181));
#19753=CARTESIAN_POINT('Ctrl Pts',(86.9756589908152,1.44154777566845,-4.19399659406254));
#19754=CARTESIAN_POINT('Ctrl Pts',(86.9699594691133,1.32063977907843,-4.23361903494679));
#19755=CARTESIAN_POINT('Ctrl Pts',(86.9642599474114,1.19836228306582,-4.26795230040417));
#19756=CARTESIAN_POINT('Ctrl Pts',(86.9585569730506,1.07601071373488,-4.30230636428306));
#19757=CARTESIAN_POINT('Ctrl Pts',(86.9528539986898,0.952288380234433,-4.33136477871307));
#19758=CARTESIAN_POINT('Ctrl Pts',(86.947151024329,0.827691978982203,-4.3550447745033));
#19759=CARTESIAN_POINT('Ctrl Pts',(86.9414398818824,0.702917124518957,-4.37875868597042));
#19760=CARTESIAN_POINT('Ctrl Pts',(86.9357287394359,0.577266096688827,-4.39707873978299));
#19761=CARTESIAN_POINT('Ctrl Pts',(86.9300175969893,0.45124108693146,-4.40997397741358));
#19762=CARTESIAN_POINT('Ctrl Pts',(86.9275147411287,0.39601178084987,-4.41562519717913));
#19763=CARTESIAN_POINT('Ctrl Pts',(86.9250118852681,0.340710657020514,-4.42023522939293));
#19764=CARTESIAN_POINT('Ctrl Pts',(86.9225090294075,0.285379884210033,-4.42380462065045));
#19765=CARTESIAN_POINT('Ctrl Pts',(86.9167978569,0.159122678004703,-4.43194948010454));
#19766=CARTESIAN_POINT('Ctrl Pts',(86.9110866843924,0.0323217523639859,
-4.43469745605847));
#19767=CARTESIAN_POINT('Ctrl Pts',(86.9053755118849,-0.0945242314710083,
-4.43199212202197));
#19768=CARTESIAN_POINT('Ctrl Pts',(86.8996713060308,-0.221215484905607,
-4.42929008803019));
#19769=CARTESIAN_POINT('Ctrl Pts',(86.8939671001767,-0.347951291536879,
-4.42114798672762));
#19770=CARTESIAN_POINT('Ctrl Pts',(86.8882628943226,-0.474228850403496,
-4.40756123014133));
#19771=CARTESIAN_POINT('Ctrl Pts',(86.8825642278143,-0.600383781320188,
-4.3939876676342));
#19772=CARTESIAN_POINT('Ctrl Pts',(86.876865561306,-0.726080955335841,-4.37498001326702));
#19773=CARTESIAN_POINT('Ctrl Pts',(86.8711668947977,-0.850819032508404,
-4.35058570469787));
#19774=CARTESIAN_POINT('Ctrl Pts',(86.8654723453115,-0.975466992210403,
-4.32620901988431));
#19775=CARTESIAN_POINT('Ctrl Pts',(86.8597777958253,-1.09915684375608,-4.29645350269457));
#19776=CARTESIAN_POINT('Ctrl Pts',(86.854083246339,-1.22139429596614,-4.26141818808966));
#19777=CARTESIAN_POINT('Ctrl Pts',(86.8483908292684,-1.34358597439709,-4.22639599302155));
#19778=CARTESIAN_POINT('Ctrl Pts',(86.8426984121977,-1.46432595181099,-4.18609804148277));
#19779=CARTESIAN_POINT('Ctrl Pts',(86.8370059951271,-1.583132349755,-4.14067397450695));
#19780=CARTESIAN_POINT('Ctrl Pts',(86.8313145092714,-1.7019193123181,-4.09525733839395));
#19781=CARTESIAN_POINT('Ctrl Pts',(86.8256230234157,-1.81877295188167,-4.0447163973388));
#19782=CARTESIAN_POINT('Ctrl Pts',(86.81993153756,-1.93322922746241,-3.98924977333898));
#19783=CARTESIAN_POINT('Ctrl Pts',(86.8142397008655,-2.04769255844206,-3.93377973022424));
#19784=CARTESIAN_POINT('Ctrl Pts',(86.808547864171,-2.15975787230553,-3.87338357435075));
#19785=CARTESIAN_POINT('Ctrl Pts',(86.8028560274765,-2.26898415615019,-3.80830669709511));
#19786=CARTESIAN_POINT('Ctrl Pts',(86.7971625579521,-2.37824177398204,-3.74321115109082));
#19787=CARTESIAN_POINT('Ctrl Pts',(86.7914690884278,-2.48465839882089,-3.67343241669553));
#19788=CARTESIAN_POINT('Ctrl Pts',(86.7857756189034,-2.58782095850807,-3.59925988040685));
#19789=CARTESIAN_POINT('Ctrl Pts',(86.7800760957878,-2.69109320596399,-3.52500848004161));
#19790=CARTESIAN_POINT('Ctrl Pts',(86.7743765726722,-2.79110415583821,-3.44635418339532));
#19791=CARTESIAN_POINT('Ctrl Pts',(86.7686770495566,-2.88747263043725,-3.36362762630999));
#19792=CARTESIAN_POINT('Ctrl Pts',(86.7629740737754,-2.98389948327371,-3.28085095500826));
#19793=CARTESIAN_POINT('Ctrl Pts',(86.7572710979942,-3.07667917421548,-3.19399738124988));
#19794=CARTESIAN_POINT('Ctrl Pts',(86.7515681222131,-3.16546743243455,-3.1034343772982));
#19795=CARTESIAN_POINT('Ctrl Pts',(86.7458569783482,-3.25438285758336,-3.01274166453825));
#19796=CARTESIAN_POINT('Ctrl Pts',(86.7401458344834,-3.33929516872905,-2.91832920924054));
#19797=CARTESIAN_POINT('Ctrl Pts',(86.7344346906186,-3.41990016645889,-2.82059778264369));
#19798=CARTESIAN_POINT('Ctrl Pts',(86.7319318498374,-3.45522434673863,-2.77776814888233));
#19799=CARTESIAN_POINT('Ctrl Pts',(86.7294290090563,-3.48972185442209,-2.73430147873475));
#19800=CARTESIAN_POINT('Ctrl Pts',(86.7269261682751,-3.52336976477716,-2.69023316845476));
#19801=CARTESIAN_POINT('Ctrl Pts',(86.7212150154459,-3.60014986196306,-2.58967509187851));
#19802=CARTESIAN_POINT('Ctrl Pts',(86.7155038626168,-3.6727441616283,-2.4856668996596));
#19803=CARTESIAN_POINT('Ctrl Pts',(86.7097927097876,-3.74082788013809,-2.3785911315696));
#19804=CARTESIAN_POINT('Ctrl Pts',(86.7040883844099,-3.8088302073252,-2.27164336821527));
#19805=CARTESIAN_POINT('Ctrl Pts',(86.6983840590322,-3.87233246567081,-2.16163565522594));
#19806=CARTESIAN_POINT('Ctrl Pts',(86.6926797336545,-3.93105046747928,-2.04898297263079));
#19807=CARTESIAN_POINT('Ctrl Pts',(86.6869809465631,-3.98971146042517,-1.93643966367071));
#19808=CARTESIAN_POINT('Ctrl Pts',(86.6812821594716,-4.04359725380571,-1.8212568445637));
#19809=CARTESIAN_POINT('Ctrl Pts',(86.6755833723802,-4.09246757400438,-1.70387738869988));
#19810=CARTESIAN_POINT('Ctrl Pts',(86.6698888386931,-4.14130141885656,-1.58658554135397));
#19811=CARTESIAN_POINT('Ctrl Pts',(86.664194305006,-4.18512708647871,-1.46710068603454));
#19812=CARTESIAN_POINT('Ctrl Pts',(86.6584997713189,-4.22375101126631,-1.34588870075753));
#19813=CARTESIAN_POINT('Ctrl Pts',(86.6528079022886,-4.26235686266863,-1.22473343449401));
#19814=CARTESIAN_POINT('Ctrl Pts',(86.6471160332582,-4.29576569288201,-1.10185302511737));
#19815=CARTESIAN_POINT('Ctrl Pts',(86.6414241642279,-4.32383285685581,-0.977731264701169));
#19816=CARTESIAN_POINT('Ctrl Pts',(86.6357339027777,-4.3518920936943,-0.853644560551788));
#19817=CARTESIAN_POINT('Ctrl Pts',(86.6300436413275,-4.37461258142881,-0.728317592141152));
#19818=CARTESIAN_POINT('Ctrl Pts',(86.6243533798773,-4.39190027218435,-0.602246626546801));
#19819=CARTESIAN_POINT('Ctrl Pts',(86.6186622188746,-4.4091906958874,-0.476155730856733));
#19820=CARTESIAN_POINT('Ctrl Pts',(86.6129710578719,-4.42104654978381,-0.349320997581811));
#19821=CARTESIAN_POINT('Ctrl Pts',(86.6072798968692,-4.42742540679828,-0.222245961126497));
#19822=CARTESIAN_POINT('Ctrl Pts',(86.6039175710256,-4.43119402198628,-0.147170299246186));
#19823=CARTESIAN_POINT('Ctrl Pts',(86.6005552451821,-4.43305191920432,-0.0720108656635592));
#19824=CARTESIAN_POINT('Ctrl Pts',(86.5971929193385,-4.43299889626848,0.00312820754919921));
#19825=CARTESIAN_POINT('',(85.3471929193076,-4.43299979596283,-0.00134498828473521));
#19826=CARTESIAN_POINT('Ctrl Pts',(86.5971929193007,-4.43299889626788,0.00312820839396158));
#19827=CARTESIAN_POINT('Ctrl Pts',(86.5906144593768,-4.4328951557713,0.150139356284962));
#19828=CARTESIAN_POINT('Ctrl Pts',(86.5840359994529,-4.42547447811461,0.296863596691938));
#19829=CARTESIAN_POINT('Ctrl Pts',(86.577457539529,-4.41084607268977,0.442635203115662));
#19830=CARTESIAN_POINT('Ctrl Pts',(86.5708439092666,-4.39613945960291,0.589186146466117));
#19831=CARTESIAN_POINT('Ctrl Pts',(86.5642302790042,-4.37414795009144,0.734774121502404));
#19832=CARTESIAN_POINT('Ctrl Pts',(86.5576166487418,-4.34503195291692,0.878741331752945));
#19833=CARTESIAN_POINT('Ctrl Pts',(86.5509627105994,-4.3157385034094,1.02358597433674));
#19834=CARTESIAN_POINT('Ctrl Pts',(86.544308772457,-4.27923354022666,1.1667899182295));
#19835=CARTESIAN_POINT('Ctrl Pts',(86.5376548343146,-4.23572891997995,1.30770391008265));
#19836=CARTESIAN_POINT('Ctrl Pts',(86.535550991924,-4.22197362765444,1.35225810087213));
#19837=CARTESIAN_POINT('Ctrl Pts',(86.5334471495333,-4.20751893789606,1.39658352669599));
#19838=CARTESIAN_POINT('Ctrl Pts',(86.5313433071426,-4.19237252860606,1.44066012001071));
#19839=CARTESIAN_POINT('Ctrl Pts',(86.5256321353073,-4.15125550076794,1.56031214311604));
#19840=CARTESIAN_POINT('Ctrl Pts',(86.519920963472,-4.10494859877901,1.67838708878222));
#19841=CARTESIAN_POINT('Ctrl Pts',(86.5142097916366,-4.05359183096115,1.79440303944377));
#19842=CARTESIAN_POINT('Ctrl Pts',(86.5085055864642,-4.00229770970667,1.91027747028398));
#19843=CARTESIAN_POINT('Ctrl Pts',(86.5028013812917,-3.94596613798181,2.0240975410831));
#19844=CARTESIAN_POINT('Ctrl Pts',(86.4970971761193,-3.88478655715426,2.13539748181774));
#19845=CARTESIAN_POINT('Ctrl Pts',(86.4913985103012,-3.82366638782589,2.24658933916493));
#19846=CARTESIAN_POINT('Ctrl Pts',(86.4856998444832,-3.757707768639,2.35526558839802));
#19847=CARTESIAN_POINT('Ctrl Pts',(86.4800011786651,-3.68714758931704,2.46098184767656));
#19848=CARTESIAN_POINT('Ctrl Pts',(86.4743066298768,-3.61663838655049,2.56662173171341));
#19849=CARTESIAN_POINT('Ctrl Pts',(86.4686120810885,-3.54153446108794,2.66930555111145));
#19850=CARTESIAN_POINT('Ctrl Pts',(86.4629175323001,-3.46211760337245,2.76861530379694));
#19851=CARTESIAN_POINT('Ctrl Pts',(86.4572251159363,-3.38273048470374,2.86788786818934));
#19852=CARTESIAN_POINT('Ctrl Pts',(86.4515326995725,-3.299033893937,2.96378856685644));
#19853=CARTESIAN_POINT('Ctrl Pts',(86.4458402832086,-3.21135154132985,3.05593034573735));
#19854=CARTESIAN_POINT('Ctrl Pts',(86.4401487980651,-3.12368353264651,3.14805705117855));
#19855=CARTESIAN_POINT('Ctrl Pts',(86.4344573129216,-3.0320313341295,3.23642577091044));
#19856=CARTESIAN_POINT('Ctrl Pts',(86.428765827778,-2.93675698656896,3.32068477905362));
#19857=CARTESIAN_POINT('Ctrl Pts',(86.4230739918002,-2.84147676611137,3.4049489810868));
#19858=CARTESIAN_POINT('Ctrl Pts',(86.4173821558224,-2.74257425155059,3.48510270324141));
#19859=CARTESIAN_POINT('Ctrl Pts',(86.4116903198446,-2.64044577389125,3.56083348601698));
#19860=CARTESIAN_POINT('Ctrl Pts',(86.4059968510407,-2.53828799847291,3.63658599380279));
#19861=CARTESIAN_POINT('Ctrl Pts',(86.4003033822368,-2.43290273943988,3.70791280043777));
#19862=CARTESIAN_POINT('Ctrl Pts',(86.394609913433,-2.3247161655013,3.77454417775934));
#19863=CARTESIAN_POINT('Ctrl Pts',(86.3889103910398,-2.2164145620233,3.84124640099427));
#19864=CARTESIAN_POINT('Ctrl Pts',(86.3832108686465,-2.10530603689519,3.90324301747818));
#19865=CARTESIAN_POINT('Ctrl Pts',(86.3775113462533,-1.9918425396822,3.96030962136956));
#19866=CARTESIAN_POINT('Ctrl Pts',(86.3718083711966,-1.87831030841598,4.01741079513661));
#19867=CARTESIAN_POINT('Ctrl Pts',(86.3661053961398,-1.76242062649897,4.06957584326114));
#19868=CARTESIAN_POINT('Ctrl Pts',(86.3604024210831,-1.64464522120501,4.11662860801986));
#19869=CARTESIAN_POINT('Ctrl Pts',(86.3546912779396,-1.52670113207099,4.16374876410723));
#19870=CARTESIAN_POINT('Ctrl Pts',(86.348980134796,-1.40686630250328,4.2057418846751));
#19871=CARTESIAN_POINT('Ctrl Pts',(86.3432689916525,-1.28562775403868,4.2424816178795));
#19872=CARTESIAN_POINT('Ctrl Pts',(86.3407661431051,-1.23249623250552,4.25858242039317));
#19873=CARTESIAN_POINT('Ctrl Pts',(86.3382632945578,-1.17909525768112,4.27367495140329));
#19874=CARTESIAN_POINT('Ctrl Pts',(86.3357604460104,-1.12546632534492,4.28775168946554));
#19875=CARTESIAN_POINT('Ctrl Pts',(86.3300492739532,-1.00309213688677,4.31987295911356));
#19876=CARTESIAN_POINT('Ctrl Pts',(86.324338101896,-0.879152957298337,4.34680069676259));
#19877=CARTESIAN_POINT('Ctrl Pts',(86.3186269298387,-0.754127476099715,
4.3683842264379));
#19878=CARTESIAN_POINT('Ctrl Pts',(86.3129227244419,-0.629254504764249,
4.38994142787095));
#19879=CARTESIAN_POINT('Ctrl Pts',(86.3072185190451,-0.503298258058655,
4.40616732349194));
#19880=CARTESIAN_POINT('Ctrl Pts',(86.3015143136482,-0.376751394775666,
4.41696132952674));
#19881=CARTESIAN_POINT('Ctrl Pts',(86.2958156476036,-0.2503274211148,4.42774485350541));
#19882=CARTESIAN_POINT('Ctrl Pts',(86.290116981559,-0.123314367625963,4.4331069504743));
#19883=CARTESIAN_POINT('Ctrl Pts',(86.2844183155143,0.00378659940249116,
4.43299838277265));
#19884=CARTESIAN_POINT('Ctrl Pts',(86.2787237664975,0.130795741746123,4.43288989350625));
#19885=CARTESIAN_POINT('Ctrl Pts',(86.2730292174807,0.25789227342292,4.42731860619702));
#19886=CARTESIAN_POINT('Ctrl Pts',(86.2673346684638,0.384572087274374,4.41628727662608));
#19887=CARTESIAN_POINT('Ctrl Pts',(86.2616422518694,0.511204463677064,4.40526007792743));
#19888=CARTESIAN_POINT('Ctrl Pts',(86.255949835275,0.637420035520863,4.3887769369016));
#19889=CARTESIAN_POINT('Ctrl Pts',(86.2502574186806,0.762717209312201,4.36689265480834));
#19890=CARTESIAN_POINT('Ctrl Pts',(86.2445659333053,0.887993885812354,4.34501195275195));
#19891=CARTESIAN_POINT('Ctrl Pts',(86.23887444793,1.01235207003775,4.31773193577678));
#19892=CARTESIAN_POINT('Ctrl Pts',(86.2331829625547,1.13529831748097,4.28515889207447));
#19893=CARTESIAN_POINT('Ctrl Pts',(86.2274911263441,1.25825214359147,4.2525838405007));
#19894=CARTESIAN_POINT('Ctrl Pts',(86.2217992901336,1.37979347395702,4.21471521550547));
#19895=CARTESIAN_POINT('Ctrl Pts',(86.216107453923,1.49944253063066,4.17170961325641));
#19896=CARTESIAN_POINT('Ctrl Pts',(86.2104139848857,1.61912591123335,4.12869167391685));
#19897=CARTESIAN_POINT('Ctrl Pts',(86.2047205158484,1.7369155627658,4.08053396067619));
#19898=CARTESIAN_POINT('Ctrl Pts',(86.1990270468111,1.85235072611109,4.02744159330408));
#19899=CARTESIAN_POINT('Ctrl Pts',(86.1933275241846,1.96790862606085,3.97429277539554));
#19900=CARTESIAN_POINT('Ctrl Pts',(86.1876280015581,2.08110667651898,3.91619899451292));
#19901=CARTESIAN_POINT('Ctrl Pts',(86.1819284789316,2.19150754275433,3.85341195436601));
#19902=CARTESIAN_POINT('Ctrl Pts',(86.1762255036414,2.30197528776012,3.79058687900988));
#19903=CARTESIAN_POINT('Ctrl Pts',(86.1705225283512,2.40964213533218,3.72306309234928));
#19904=CARTESIAN_POINT('Ctrl Pts',(86.164819553061,2.51409993842635,3.65113550825009));
#19905=CARTESIAN_POINT('Ctrl Pts',(86.1591084096857,2.61870735118599,3.57910490588441));
#19906=CARTESIAN_POINT('Ctrl Pts',(86.1533972663104,2.72009622403066,3.50265815158753));
#19907=CARTESIAN_POINT('Ctrl Pts',(86.1476861229351,2.81789137980966,3.42213050183572));
#19908=CARTESIAN_POINT('Ctrl Pts',(86.145183276916,2.8607490354903,3.38684014150711));
#19909=CARTESIAN_POINT('Ctrl Pts',(86.142680430897,2.90291698057388,3.35076651150491));
#19910=CARTESIAN_POINT('Ctrl Pts',(86.140177584878,2.94436594871412,3.31393997532436));
#19911=CARTESIAN_POINT('Ctrl Pts',(86.1344664130515,3.03894714838806,3.2299065692331));
#19912=CARTESIAN_POINT('Ctrl Pts',(86.128755241225,3.1300738605265,3.14169123977798));
#19913=CARTESIAN_POINT('Ctrl Pts',(86.1230440693985,3.21735528449407,3.04960882300305));
#19914=CARTESIAN_POINT('Ctrl Pts',(86.1173398642333,3.30453023992418,2.95763873116275));
#19915=CARTESIAN_POINT('Ctrl Pts',(86.111635659068,3.38786896680283,2.86181122398429));
#19916=CARTESIAN_POINT('Ctrl Pts',(86.1059314539028,3.46701460729642,2.7624805361836));
#19917=CARTESIAN_POINT('Ctrl Pts',(86.1002327880902,3.54608338947103,2.66324630839815));
#19918=CARTESIAN_POINT('Ctrl Pts',(86.0945341222777,3.6209669404316,2.56051597977903));
#19919=CARTESIAN_POINT('Ctrl Pts',(86.0888354564652,3.69134641690937,2.45467933351189));
#19920=CARTESIAN_POINT('Ctrl Pts',(86.0831409076808,3.76167504740151,2.34891914943038));
#19921=CARTESIAN_POINT('Ctrl Pts',(86.0774463588963,3.82750585956527,2.24005744552949));
#19922=CARTESIAN_POINT('Ctrl Pts',(86.0717518101118,3.88856164977795,2.12851527969056));
#19923=CARTESIAN_POINT('Ctrl Pts',(86.0660593937494,3.94959457659708,2.01701488273918));
#19924=CARTESIAN_POINT('Ctrl Pts',(86.0603669773869,4.005855845439,1.90283636919786));
#19925=CARTESIAN_POINT('Ctrl Pts',(86.0546745610245,4.05711295984482,1.78642756110042));
#19926=CARTESIAN_POINT('Ctrl Pts',(86.0489830758808,4.10836168913209,1.67003779624543));
#19927=CARTESIAN_POINT('Ctrl Pts',(86.0432915907371,4.15460773150647,1.55141882773757));
#19928=CARTESIAN_POINT('Ctrl Pts',(86.0376001055934,4.19566595728358,1.43104024223349));
#19929=CARTESIAN_POINT('Ctrl Pts',(86.0319082696138,4.23672671398111,1.31065423632547));
#19930=CARTESIAN_POINT('Ctrl Pts',(86.0262164336343,4.27259888919706,1.18850877549396));
#19931=CARTESIAN_POINT('Ctrl Pts',(86.0205245976548,4.30314679802921,1.06508996550101));
#19932=CARTESIAN_POINT('Ctrl Pts',(86.0148311288477,4.33370347019691,0.941635750124001));
#19933=CARTESIAN_POINT('Ctrl Pts',(86.0091376600406,4.35893274162317,0.816907846213275));
#19934=CARTESIAN_POINT('Ctrl Pts',(86.0034441912335,4.3787498547006,0.691403435021481));
#19935=CARTESIAN_POINT('Ctrl Pts',(85.9977446688347,4.3985880383617,0.565765581022593));
#19936=CARTESIAN_POINT('Ctrl Pts',(85.9920451464359,4.41300251188449,0.439349965915013));
#19937=CARTESIAN_POINT('Ctrl Pts',(85.9863456240371,4.42196027333882,0.312660104607597));
#19938=CARTESIAN_POINT('Ctrl Pts',(85.9806426489735,4.4309234612387,0.18589349693477));
#19939=CARTESIAN_POINT('Ctrl Pts',(85.9749396739098,4.43442334099854,0.058852710456793));
#19940=CARTESIAN_POINT('Ctrl Pts',(85.9692366988462,4.43247905402526,-0.0679590731790049));
#19941=CARTESIAN_POINT('Ctrl Pts',(85.9635255556938,4.43053198234603,-0.194952483052602));
#19942=CARTESIAN_POINT('Ctrl Pts',(85.9578144125414,4.4231251975759,-0.321715837576687));
#19943=CARTESIAN_POINT('Ctrl Pts',(85.952103269389,4.41032969502454,-0.447751025889136));
#19944=CARTESIAN_POINT('Ctrl Pts',(85.9496004208412,4.40472220032081,-0.50298462442174));
#19945=CARTESIAN_POINT('Ctrl Pts',(85.9470975722934,4.39808044483649,-0.558078504930061));
#19946=CARTESIAN_POINT('Ctrl Pts',(85.9445947237456,4.3904134714002,-0.612991476407032));
#19947=CARTESIAN_POINT('Ctrl Pts',(85.9388835519819,4.37291844468733,-0.738295667279145));
#19948=CARTESIAN_POINT('Ctrl Pts',(85.9331723802182,4.35002781647401,-0.863043575908686));
#19949=CARTESIAN_POINT('Ctrl Pts',(85.9274612084545,4.32178692539746,-0.986735411072074));
#19950=CARTESIAN_POINT('Ctrl Pts',(85.9217570033536,4.29358048342722,-1.11027636313593));
#19951=CARTESIAN_POINT('Ctrl Pts',(85.9160527982526,4.26003685086349,-1.23276341883413));
#19952=CARTESIAN_POINT('Ctrl Pts',(85.9103485931516,4.22125297409735,-1.35370319076018));
#19953=CARTESIAN_POINT('Ctrl Pts',(85.9046499274048,4.18250676035782,-1.47452551806159));
#19954=CARTESIAN_POINT('Ctrl Pts',(85.898951261658,4.13853054960645,-1.59380317353583));
#19955=CARTESIAN_POINT('Ctrl Pts',(85.8932525959112,4.08947194930563,-1.7110546969172));
#19956=CARTESIAN_POINT('Ctrl Pts',(85.8875580471937,4.04044879163431,-1.82822151135302));
#19957=CARTESIAN_POINT('Ctrl Pts',(85.8818634984763,3.98635070594406,-1.94336474011074));
#19958=CARTESIAN_POINT('Ctrl Pts',(85.8761689497589,3.92737441392121,-2.05602023649501));
#19959=CARTESIAN_POINT('Ctrl Pts',(85.8704765334651,3.86842020660578,-2.16863354705188));
#19960=CARTESIAN_POINT('Ctrl Pts',(85.8647841171714,3.80459160993615,-2.27876062446177));
#19961=CARTESIAN_POINT('Ctrl Pts',(85.8590917008776,3.73613240679481,-2.38595968928598));
#19962=CARTESIAN_POINT('Ctrl Pts',(85.8534002158037,3.66768440286324,-2.49314121746413));
#19963=CARTESIAN_POINT('Ctrl Pts',(85.8477087307297,3.59460751399057,-2.59739534952529));
#19964=CARTESIAN_POINT('Ctrl Pts',(85.8420172456557,3.51718989812161,-2.69830765861702));
#19965=CARTESIAN_POINT('Ctrl Pts',(85.8363254097469,3.43976751007137,-2.79922618815132));
#19966=CARTESIAN_POINT('Ctrl Pts',(85.8306335738381,3.35800410582481,-2.89680216830276));
#19967=CARTESIAN_POINT('Ctrl Pts',(85.8249417379292,3.27222900507449,-2.99065316249631));
#19968=CARTESIAN_POINT('Ctrl Pts',(85.8192482691937,3.18642929787401,-3.08453107988542));
#19969=CARTESIAN_POINT('Ctrl Pts',(85.8135548004581,3.09661587392479,-3.17468159099211));
#19970=CARTESIAN_POINT('Ctrl Pts',(85.8078613317226,3.00315550632496,-3.26075850145792));
#19971=CARTESIAN_POINT('Ctrl Pts',(85.8021618093963,2.90959576682281,-3.34692693335209));
#19972=CARTESIAN_POINT('Ctrl Pts',(85.7964622870699,2.8123816354345,-3.42901284610396));
#19973=CARTESIAN_POINT('Ctrl Pts',(85.7907627647436,2.7119138516841,-3.50670960603297));
#19974=CARTESIAN_POINT('Ctrl Pts',(85.7850597897531,2.61138520642603,-3.58445343320856));
#19975=CARTESIAN_POINT('Ctrl Pts',(85.7793568147625,2.50759930776965,-3.6578025807879));
#19976=CARTESIAN_POINT('Ctrl Pts',(85.773653839772,2.40098552823103,-3.72649399479258));
#19977=CARTESIAN_POINT('Ctrl Pts',(85.767942696693,2.29421905105937,-3.79528379210543));
#19978=CARTESIAN_POINT('Ctrl Pts',(85.762231553614,2.18461694940847,-3.85940233424258));
#19979=CARTESIAN_POINT('Ctrl Pts',(85.756520410535,2.07263312563219,-3.91863253272518));
#19980=CARTESIAN_POINT('Ctrl Pts',(85.7540175612277,2.02355737461579,-3.94458955379628));
#19981=CARTESIAN_POINT('Ctrl Pts',(85.7515147119205,1.97402446467942,-3.96960837257711));
#19982=CARTESIAN_POINT('Ctrl Pts',(85.7490118626132,1.92407368970206,-3.99367367677885));
#19983=CARTESIAN_POINT('Ctrl Pts',(85.7433006900686,1.81009259870891,-4.04858753205416));
#19984=CARTESIAN_POINT('Ctrl Pts',(85.7375895175239,1.6935829226719,-4.09870261257304));
#19985=CARTESIAN_POINT('Ctrl Pts',(85.7318783449793,1.57498573745547,-4.1437795461163));
#19986=CARTESIAN_POINT('Ctrl Pts',(85.7261741390951,1.45653322066087,-4.18880149345712));
#19987=CARTESIAN_POINT('Ctrl Pts',(85.7204699332109,1.33599863063617,-4.22879737994613));
#19988=CARTESIAN_POINT('Ctrl Pts',(85.7147657273267,1.21384632721907,-4.26357433310324));
#19989=CARTESIAN_POINT('Ctrl Pts',(85.7090670607953,1.09181264587102,-4.29831751437048));
#19990=CARTESIAN_POINT('Ctrl Pts',(85.7033683942639,0.968164758856482,-4.32785173842749));
#19991=CARTESIAN_POINT('Ctrl Pts',(85.6976697277325,0.843385188467329,-4.35203290703022));
#19992=CARTESIAN_POINT('Ctrl Pts',(85.6919751782301,0.718695765677514,-4.37619660583167));
#19993=CARTESIAN_POINT('Ctrl Pts',(85.6862806287277,0.59287667729466,-4.39501487067645));
#19994=CARTESIAN_POINT('Ctrl Pts',(85.6805860792253,0.466423267717234,-4.4083940766828));
#19995=CARTESIAN_POINT('Ctrl Pts',(85.6748936621488,0.34001721088171,-4.42176827260605));
#19996=CARTESIAN_POINT('Ctrl Pts',(85.6692012450724,0.212977701444396,-4.42970741750697));
#19997=CARTESIAN_POINT('Ctrl Pts',(85.6635088279959,0.0858075618328727,
-4.43216945325112));
#19998=CARTESIAN_POINT('Ctrl Pts',(85.6578173421409,-0.0413417740395733,
-4.4346310862313));
#19999=CARTESIAN_POINT('Ctrl Pts',(85.6521258562858,-0.168621298641298,
-4.4316173845517));
#20000=CARTESIAN_POINT('Ctrl Pts',(85.6464343704308,-0.295526349723232,
-4.42313838542491));
#20001=CARTESIAN_POINT('Ctrl Pts',(85.6407425337434,-0.422439223437343,
-4.41465886363893));
#20002=CARTESIAN_POINT('Ctrl Pts',(85.635050697056,-0.54897717943748,-4.4007134009788));
#20003=CARTESIAN_POINT('Ctrl Pts',(85.6293588603686,-0.674639356838034,
-4.3813640271273));
#20004=CARTESIAN_POINT('Ctrl Pts',(85.6236653908578,-0.800337583084492,
-4.36200910249982));
#20005=CARTESIAN_POINT('Ctrl Pts',(85.617971921347,-0.925159136584635,-4.33724724346669));
#20006=CARTESIAN_POINT('Ctrl Pts',(85.6122784518362,-1.04861255243217,-4.30719174345439));
#20007=CARTESIAN_POINT('Ctrl Pts',(85.6065789287439,-1.17219723012678,-4.27710428693106));
#20008=CARTESIAN_POINT('Ctrl Pts',(85.6008794056515,-1.29441047758078,-4.24171204607327));
#20009=CARTESIAN_POINT('Ctrl Pts',(85.5951798825591,-1.41477492088964,-4.20117851599069));
#20010=CARTESIAN_POINT('Ctrl Pts',(85.5894769068067,-1.53521227863213,-4.16062043148565));
#20011=CARTESIAN_POINT('Ctrl Pts',(85.5837739310544,-1.65379822927678,-4.11491499663148));
#20012=CARTESIAN_POINT('Ctrl Pts',(85.578070955302,-1.77007579171369,-4.06427369791814));
#20013=CARTESIAN_POINT('Ctrl Pts',(85.5723598114742,-1.88651989245249,-4.01355986830789));
#20014=CARTESIAN_POINT('Ctrl Pts',(85.5666486676464,-2.0006486453519,-3.95789623353993));
#20015=CARTESIAN_POINT('Ctrl Pts',(85.5609375238187,-2.1120297225665,-3.89754017952293));
#20016=CARTESIAN_POINT('Ctrl Pts',(85.5584346830394,-2.16084115342805,-3.87108985751671));
#20017=CARTESIAN_POINT('Ctrl Pts',(85.5559318422602,-2.20912526059895,-3.84373890644368));
#20018=CARTESIAN_POINT('Ctrl Pts',(85.5534290014809,-2.25684751509205,-3.8155115376084));
#20019=CARTESIAN_POINT('Ctrl Pts',(85.5477178303485,-2.3657437599082,-3.75110019535618));
#20020=CARTESIAN_POINT('Ctrl Pts',(85.5420066592161,-2.47204829966788,-3.68192387470062));
#20021=CARTESIAN_POINT('Ctrl Pts',(85.5362954880837,-2.57531737322834,-3.60821693183049));
#20022=CARTESIAN_POINT('Ctrl Pts',(85.5305912836099,-2.67846047606241,-3.53459989890933));
#20023=CARTESIAN_POINT('Ctrl Pts',(85.5248870791361,-2.77857515714656,-3.45646346872346));
#20024=CARTESIAN_POINT('Ctrl Pts',(85.5191828746622,-2.87524344395868,-3.37408715625021));
#20025=CARTESIAN_POINT('Ctrl Pts',(85.5134842095377,-2.97181785625936,-3.29179083936127));
#20026=CARTESIAN_POINT('Ctrl Pts',(85.5077855444132,-3.06495223182522,-3.20526309055057));
#20027=CARTESIAN_POINT('Ctrl Pts',(85.5020868792887,-3.15425911922232,-3.11482558240471));
#20028=CARTESIAN_POINT('Ctrl Pts',(85.4963923311881,-3.24350148649438,-3.02445341120546));
#20029=CARTESIAN_POINT('Ctrl Pts',(85.4906977830874,-3.32892158964286,-2.93017738557085));
#20030=CARTESIAN_POINT('Ctrl Pts',(85.4850032349868,-3.41016687327916,-2.83235783339419));
#20031=CARTESIAN_POINT('Ctrl Pts',(85.4793108192995,-3.49138173333796,-2.73457491129122));
#20032=CARTESIAN_POINT('Ctrl Pts',(85.4736184036121,-3.56842462768289,-2.63325140758664));
#20033=CARTESIAN_POINT('Ctrl Pts',(85.4679259879248,-3.6409817698824,-2.5287824642274));
#20034=CARTESIAN_POINT('Ctrl Pts',(85.4622345034506,-3.71352704257538,-2.42433061077508));
#20035=CARTESIAN_POINT('Ctrl Pts',(85.4565430189765,-3.78158779513353,-2.31673466889177));
#20036=CARTESIAN_POINT('Ctrl Pts',(85.4508515345023,-3.84489257604527,-2.20642019540068));
#20037=CARTESIAN_POINT('Ctrl Pts',(85.445159699186,-3.90820125927502,-2.09609892175721));
#20038=CARTESIAN_POINT('Ctrl Pts',(85.4394678638698,-3.96675318908799,-1.98305912942441));
#20039=CARTESIAN_POINT('Ctrl Pts',(85.4337760285535,-4.02032229097474,-1.86775203833154));
#20040=CARTESIAN_POINT('Ctrl Pts',(85.4280825604026,-4.07390676039728,-1.75241186873282));
#20041=CARTESIAN_POINT('Ctrl Pts',(85.4223890922517,-4.12250539013308,-1.63480346830541));
#20042=CARTESIAN_POINT('Ctrl Pts',(85.4166956241009,-4.16593997808967,-1.51539866007405));
#20043=CARTESIAN_POINT('Ctrl Pts',(85.4109961023443,-4.20942074806791,-1.39586689414151));
#20044=CARTESIAN_POINT('Ctrl Pts',(85.4052965805877,-4.2477263769179,-1.2745352822411));
#20045=CARTESIAN_POINT('Ctrl Pts',(85.3995970588311,-4.28072825419882,-1.15189175433453));
#20046=CARTESIAN_POINT('Ctrl Pts',(85.3938940844026,-4.31375012344783,-1.02917393109399));
#20047=CARTESIAN_POINT('Ctrl Pts',(85.388191109974,-4.34146175371432,-0.905142997552945));
#20048=CARTESIAN_POINT('Ctrl Pts',(85.3824881355455,-4.36378578070761,-0.78029652062154));
#20049=CARTESIAN_POINT('Ctrl Pts',(85.3767769930118,-4.386141781367,-0.655271231884875));
#20050=CARTESIAN_POINT('Ctrl Pts',(85.371065850478,-4.40309471772306,-0.529428462110429));
#20051=CARTESIAN_POINT('Ctrl Pts',(85.3653547079443,-4.41461909282753,-0.403270709626425));
#20052=CARTESIAN_POINT('Ctrl Pts',(85.362851852079,-4.41966954458104,-0.347983231001733));
#20053=CARTESIAN_POINT('Ctrl Pts',(85.3603489962138,-4.42367808959139,-0.292635258380975));
#20054=CARTESIAN_POINT('Ctrl Pts',(85.3578461403485,-4.42664573287411,-0.237268952093333));
#20055=CARTESIAN_POINT('Ctrl Pts',(85.3542950666785,-4.43085625097439,-0.15871475518988));
#20056=CARTESIAN_POINT('Ctrl Pts',(85.3507439930085,-4.4329759173203,-0.0800475054487878));
#20057=CARTESIAN_POINT('Ctrl Pts',(85.3471929193385,-4.43299979596262,-0.00134498896944356));
#20058=CARTESIAN_POINT('',(84.0971929193621,-4.43299983598826,-0.00120587233263061));
#20059=CARTESIAN_POINT('Ctrl Pts',(85.3471929193076,-4.43299979596283,-0.00134498828473226));
#20060=CARTESIAN_POINT('Ctrl Pts',(85.3415282140113,-4.43303788737273,0.124201988030421));
#20061=CARTESIAN_POINT('Ctrl Pts',(85.3358635087149,-4.42773831151435,0.249954571554026));
#20062=CARTESIAN_POINT('Ctrl Pts',(85.3301988034186,-4.41707483986748,0.375418245440573));
#20063=CARTESIAN_POINT('Ctrl Pts',(85.3245408265264,-4.4064240340422,0.500732896517129));
#20064=CARTESIAN_POINT('Ctrl Pts',(85.3188828496342,-4.39042203787962,0.625758919050579));
#20065=CARTESIAN_POINT('Ctrl Pts',(85.313224872742,-4.36909462571147,0.750000767719023));
#20066=CARTESIAN_POINT('Ctrl Pts',(85.3075721479842,-4.34778701115638,0.874127286312468));
#20067=CARTESIAN_POINT('Ctrl Pts',(85.3019194232265,-4.32116388290341,0.997470680771747));
#20068=CARTESIAN_POINT('Ctrl Pts',(85.2962666984688,-4.28930285940635,1.11954007533831));
#20069=CARTESIAN_POINT('Ctrl Pts',(85.2906175557129,-4.25746202550785,1.24153211733417));
#20070=CARTESIAN_POINT('Ctrl Pts',(85.284968412957,-4.2203900012271,1.36225137334623));
#20071=CARTESIAN_POINT('Ctrl Pts',(85.2793192702011,-4.17821546973224,1.4812172320393));
#20072=CARTESIAN_POINT('Ctrl Pts',(85.2736719911722,-4.13605485217438,1.6001438423186));
#20073=CARTESIAN_POINT('Ctrl Pts',(85.2680247121434,-4.0887952099321,1.71731782282565));
#20074=CARTESIAN_POINT('Ctrl Pts',(85.2623774331146,-4.03661490893153,1.83227429087233));
#20075=CARTESIAN_POINT('Ctrl Pts',(85.2567306908283,-3.98443956737916,1.94721983294431));
#20076=CARTESIAN_POINT('Ctrl Pts',(85.251083948542,-3.92734466520962,2.0599479117584));
#20077=CARTESIAN_POINT('Ctrl Pts',(85.2454372062557,-3.86555623384926,2.1700147471732));
#20078=CARTESIAN_POINT('Ctrl Pts',(85.239789674387,-3.8037591626301,2.28009697320231));
#20079=CARTESIAN_POINT('Ctrl Pts',(85.2341421425184,-3.73726745645285,2.3875168617243));
#20080=CARTESIAN_POINT('Ctrl Pts',(85.2284946106497,-3.66635220006584,2.49185684682576));
#20081=CARTESIAN_POINT('Ctrl Pts',(85.2228415718791,-3.5953677942917,2.59629857372989));
#20082=CARTESIAN_POINT('Ctrl Pts',(85.2171885331084,-3.51995145158518,2.69765406196533));
#20083=CARTESIAN_POINT('Ctrl Pts',(85.2115354943378,-3.44041671265339,2.79553605651854));
#20084=CARTESIAN_POINT('Ctrl Pts',(85.2058796766761,-3.36084287645444,2.89346616738599));
#20085=CARTESIAN_POINT('Ctrl Pts',(85.2002238590145,-3.2771468807361,2.98791907923903));
#20086=CARTESIAN_POINT('Ctrl Pts',(85.1945680413529,-3.18968041661611,3.07854313594201));
#20087=CARTESIAN_POINT('Ctrl Pts',(85.1889034265582,-3.10207790600888,3.16930815049322));
#20088=CARTESIAN_POINT('Ctrl Pts',(85.1832388117635,-3.01069350446996,3.25623213115127));
#20089=CARTESIAN_POINT('Ctrl Pts',(85.1775741969688,-2.91591382201898,3.33900218367084));
#20090=CARTESIAN_POINT('Ctrl Pts',(85.1724705577179,-2.83052031776918,3.41357539017258));
#20091=CARTESIAN_POINT('Ctrl Pts',(85.167366918467,-2.74237132042908,3.48477708333452));
#20092=CARTESIAN_POINT('Ctrl Pts',(85.1622632792161,-2.65176930431954,3.55240883861481));
#20093=CARTESIAN_POINT('Ctrl Pts',(85.1565521021975,-2.55038201442544,3.62809148534929));
#20094=CARTESIAN_POINT('Ctrl Pts',(85.1508409251788,-2.44559573299975,3.69954696648941));
#20095=CARTESIAN_POINT('Ctrl Pts',(85.1451297481602,-2.33779766712063,3.76645603553332));
#20096=CARTESIAN_POINT('Ctrl Pts',(85.1394255377919,-2.23013109627913,3.83328348705951));
#20097=CARTESIAN_POINT('Ctrl Pts',(85.1337213274237,-2.11946038629147,3.89557535113553));
#20098=CARTESIAN_POINT('Ctrl Pts',(85.1280171170554,-2.00620448474273,3.95305357482012));
#20099=CARTESIAN_POINT('Ctrl Pts',(85.1223184460353,-1.8930585657898,4.01047598150836));
#20100=CARTESIAN_POINT('Ctrl Pts',(85.1166197750152,-1.77733280469662,4.06309386980102));
#20101=CARTESIAN_POINT('Ctrl Pts',(85.110921103995,-1.65947329705126,4.11067359156305));
#20102=CARTESIAN_POINT('Ctrl Pts',(85.1052265500045,-1.54169893751839,4.15821893914871));
#20103=CARTESIAN_POINT('Ctrl Pts',(85.0995319960139,-1.4217942684245,4.20073321568559));
#20104=CARTESIAN_POINT('Ctrl Pts',(85.0938374420234,-1.30022761611469,4.23802986613978));
#20105=CARTESIAN_POINT('Ctrl Pts',(85.0881450204762,-1.17870648694803,4.27531255009307));
#20106=CARTESIAN_POINT('Ctrl Pts',(85.082452598929,-1.05552499301529,4.30738137598142));
#20107=CARTESIAN_POINT('Ctrl Pts',(85.0767601773817,-0.931168654758774,
4.33409897630346));
#20108=CARTESIAN_POINT('Ctrl Pts',(85.0710686870681,-0.806832660181519,
4.36081220584474));
#20109=CARTESIAN_POINT('Ctrl Pts',(85.0653771967545,-0.681322593683535,
4.3821758672857));
#20110=CARTESIAN_POINT('Ctrl Pts',(85.0596857064408,-0.55513573651598,4.39810337691633));
#20111=CARTESIAN_POINT('Ctrl Pts',(85.0539938653117,-0.428941101368054,
4.41403186829625));
#20112=CARTESIAN_POINT('Ctrl Pts',(85.0483020241826,-0.302069988610285,
4.42452349144645));
#20113=CARTESIAN_POINT('Ctrl Pts',(85.0426101830535,-0.175025883421164,
4.42954342343911));
#20114=CARTESIAN_POINT('Ctrl Pts',(85.0369167091228,-0.0479453334641138,
4.43456479548485));
#20115=CARTESIAN_POINT('Ctrl Pts',(85.031223235192,0.0793079089593364,4.43411133804602));
#20116=CARTESIAN_POINT('Ctrl Pts',(85.0255297612612,0.206229785507273,4.42820034275434));
#20117=CARTESIAN_POINT('Ctrl Pts',(85.0198302338054,0.333286610378385,4.42228306266034));
#20118=CARTESIAN_POINT('Ctrl Pts',(85.0141307063495,0.46001096684867,4.41089667762191));
#20119=CARTESIAN_POINT('Ctrl Pts',(85.0084311788937,0.585903034864924,4.39411044851356));
#20120=CARTESIAN_POINT('Ctrl Pts',(85.0027281988043,0.71187136520028,4.3773140507204));
#20121=CARTESIAN_POINT('Ctrl Pts',(84.9970252187149,0.837006010321613,4.35511136207105));
#20122=CARTESIAN_POINT('Ctrl Pts',(84.9913222386254,0.960817996480046,4.32762264732498));
#20123=CARTESIAN_POINT('Ctrl Pts',(84.9856110905386,1.08480731027524,4.3000945623291));
#20124=CARTESIAN_POINT('Ctrl Pts',(84.9798999424518,1.20746979779887,4.26726543705814));
#20125=CARTESIAN_POINT('Ctrl Pts',(84.974188794365,1.32833191332227,4.22930530087975));
#20126=CARTESIAN_POINT('Ctrl Pts',(84.9716860022713,1.3812972265245,4.2126700591981));
#20127=CARTESIAN_POINT('Ctrl Pts',(84.9691832101775,1.43391704778814,4.19505005678398));
#20128=CARTESIAN_POINT('Ctrl Pts',(84.9666804180838,1.486152860131,4.1764624595852));
#20129=CARTESIAN_POINT('Ctrl Pts',(84.960969254316,1.6053506471065,4.13404710598173));
#20130=CARTESIAN_POINT('Ctrl Pts',(84.9552580905483,1.72291503430886,4.0864593429778));
#20131=CARTESIAN_POINT('Ctrl Pts',(84.9495469267805,1.83836565569993,4.03384440899038));
#20132=CARTESIAN_POINT('Ctrl Pts',(84.9438427296566,1.95367544706221,3.98129365623108));
#20133=CARTESIAN_POINT('Ctrl Pts',(84.9381385325326,2.06687624225092,3.92372809667851));
#20134=CARTESIAN_POINT('Ctrl Pts',(84.9324343354087,2.177504359174,3.86134222334388));
#20135=CARTESIAN_POINT('Ctrl Pts',(84.926735677611,2.28802504551298,3.79901693271641));
#20136=CARTESIAN_POINT('Ctrl Pts',(84.9210370198133,2.39597767915769,3.73188083776983));
#20137=CARTESIAN_POINT('Ctrl Pts',(84.9153383620155,2.50092048073354,3.66017564456236));
#20138=CARTESIAN_POINT('Ctrl Pts',(84.9096438212103,2.60578746643538,3.58852225473552));
#20139=CARTESIAN_POINT('Ctrl Pts',(84.903949280405,2.7076486194383,3.51230656094385));
#20140=CARTESIAN_POINT('Ctrl Pts',(84.8982547395997,2.80608902669326,3.43181488053649));
#20141=CARTESIAN_POINT('Ctrl Pts',(84.8925623311348,2.90449257259949,3.35135334051542));
#20142=CARTESIAN_POINT('Ctrl Pts',(84.8868699226699,2.99947761112639,3.26661924977286));
#20143=CARTESIAN_POINT('Ctrl Pts',(84.881177514205,3.09066063112659,3.17794050655518));
#20144=CARTESIAN_POINT('Ctrl Pts',(84.8754860369058,3.18182873538483,3.08927626942922));
#20145=CARTESIAN_POINT('Ctrl Pts',(84.8697945596065,3.26919577215273,2.99666894151143));
#20146=CARTESIAN_POINT('Ctrl Pts',(84.8641030823072,3.35241397309439,2.90048436523997));
#20147=CARTESIAN_POINT('Ctrl Pts',(84.8584112541108,3.43563730469505,2.80429385889244));
#20148=CARTESIAN_POINT('Ctrl Pts',(84.8527194259144,3.51471103055647,2.70452596741517));
#20149=CARTESIAN_POINT('Ctrl Pts',(84.847027597718,3.58932701920446,2.60158039453114));
#20150=CARTESIAN_POINT('Ctrl Pts',(84.8413341366245,3.66396441402169,2.49860528815978));
#20151=CARTESIAN_POINT('Ctrl Pts',(84.8356406755309,3.7341412933782,2.39245100990343));
#20152=CARTESIAN_POINT('Ctrl Pts',(84.8299472144373,3.79959257901694,2.28354663483787));
#20153=CARTESIAN_POINT('Ctrl Pts',(84.8242476996059,3.86511345763529,2.17452646403387));
#20154=CARTESIAN_POINT('Ctrl Pts',(84.8185481847745,3.92589850451247,2.06275070051456));
#20155=CARTESIAN_POINT('Ctrl Pts',(84.8128486699432,3.98172824133116,1.94867370593075));
#20156=CARTESIAN_POINT('Ctrl Pts',(84.8071457023737,4.03759179953024,1.83452760406385));
#20157=CARTESIAN_POINT('Ctrl Pts',(84.8014427348042,4.08849390791508,1.7180778591149));
#20158=CARTESIAN_POINT('Ctrl Pts',(84.7957397672347,4.13426354847867,1.59979808467211));
#20159=CARTESIAN_POINT('Ctrl Pts',(84.7900286313998,4.18009874413595,1.48134890007885));
#20160=CARTESIAN_POINT('Ctrl Pts',(84.7843174955649,4.22078666584669,1.36106482950147));
#20161=CARTESIAN_POINT('Ctrl Pts',(84.77860635973,4.25620626483195,1.23943423835443));
#20162=CARTESIAN_POINT('Ctrl Pts',(84.7761034254704,4.27172908381607,1.18612901459703));
#20163=CARTESIAN_POINT('Ctrl Pts',(84.7736004912109,4.28624069249104,1.13256529713689));
#20164=CARTESIAN_POINT('Ctrl Pts',(84.7710975569514,4.29973402033953,1.07878466541515));
#20165=CARTESIAN_POINT('Ctrl Pts',(84.765386387843,4.33052295412135,0.956068584740487));
#20166=CARTESIAN_POINT('Ctrl Pts',(84.7596752187347,4.35610165707599,0.831844066722693));
#20167=CARTESIAN_POINT('Ctrl Pts',(84.7539640496263,4.37632466568423,0.706591409885409));
#20168=CARTESIAN_POINT('Ctrl Pts',(84.7482598472653,4.39652300533454,0.58149154201145));
#20169=CARTESIAN_POINT('Ctrl Pts',(84.7425556449042,4.41137858508747,0.455366421148501));
#20170=CARTESIAN_POINT('Ctrl Pts',(84.7368514425432,4.42079618250531,0.328709769776476));
#20171=CARTESIAN_POINT('Ctrl Pts',(84.7311527796165,4.43020463435658,0.202176116530777));
#20172=CARTESIAN_POINT('Ctrl Pts',(84.7254541166898,4.43418558268488,0.0751123557100857));
#20173=CARTESIAN_POINT('Ctrl Pts',(84.719755453763,4.43269524060635,-0.0519798413408479));
#20174=CARTESIAN_POINT('Ctrl Pts',(84.7140609079416,4.43120597525325,-0.178980218263863));
#20175=CARTESIAN_POINT('Ctrl Pts',(84.7083663621202,4.42425329149755,-0.30600859275918));
#20176=CARTESIAN_POINT('Ctrl Pts',(84.7026718162988,4.41184542479171,-0.432560917957741));
#20177=CARTESIAN_POINT('Ctrl Pts',(84.6969794030022,4.39944220465206,-0.559065851145361));
#20178=CARTESIAN_POINT('Ctrl Pts',(84.6912869897057,4.38158790239047,-0.685094692894899));
#20179=CARTESIAN_POINT('Ctrl Pts',(84.6855945764091,4.35834276853733,-0.810146475606956));
#20180=CARTESIAN_POINT('Ctrl Pts',(84.6799030943942,4.33510143759976,-0.935177799784545));
#20181=CARTESIAN_POINT('Ctrl Pts',(84.6742116123793,4.30647110225273,-1.05923199058084));
#20182=CARTESIAN_POINT('Ctrl Pts',(84.6685201303644,4.27256340833325,-1.18181678858092));
#20183=CARTESIAN_POINT('Ctrl Pts',(84.6628282975729,4.23865362461961,-1.30440914170987));
#20184=CARTESIAN_POINT('Ctrl Pts',(84.6571364647814,4.19946594185683,-1.42553153719938));
#20185=CARTESIAN_POINT('Ctrl Pts',(84.6514446319899,4.15516216232301,-1.54470592825922));
#20186=CARTESIAN_POINT('Ctrl Pts',(84.6457511664263,4.11084567370657,-1.66391450595501));
#20187=CARTESIAN_POINT('Ctrl Pts',(84.6400577008628,4.06141030775849,-1.78117359356347));
#20188=CARTESIAN_POINT('Ctrl Pts',(84.6343642352992,4.00706618074523,-1.89602468948266));
#20189=CARTESIAN_POINT('Ctrl Pts',(84.6286647162093,3.95266427282489,-2.01099789980257));
#20190=CARTESIAN_POINT('Ctrl Pts',(84.6229651971194,3.89334335400322,-2.12355764543186));
#20191=CARTESIAN_POINT('Ctrl Pts',(84.6172656780295,3.82935986709181,-2.23326935417709));
#20192=CARTESIAN_POINT('Ctrl Pts',(84.6115627063165,3.76533762061858,-2.34304752347276));
#20193=CARTESIAN_POINT('Ctrl Pts',(84.6058597346035,3.696647394774,-2.44997388366463));
#20194=CARTESIAN_POINT('Ctrl Pts',(84.6001567628905,3.62358852267693,-2.55364351825466));
#20195=CARTESIAN_POINT('Ctrl Pts',(84.594445623123,3.55042501235113,-2.65746163319519));
#20196=CARTESIAN_POINT('Ctrl Pts',(84.5887344833553,3.47288060528993,-2.75801339338908));
#20197=CARTESIAN_POINT('Ctrl Pts',(84.5830233435877,3.39129461642376,-2.85492728884909));
#20198=CARTESIAN_POINT('Ctrl Pts',(84.5805204609982,3.35553990556104,-2.89739938925394));
#20199=CARTESIAN_POINT('Ctrl Pts',(84.5780175784086,3.31900944650053,-2.93917328425464));
#20200=CARTESIAN_POINT('Ctrl Pts',(84.575514695819,3.28173392048605,-2.98022003803935));
#20201=CARTESIAN_POINT('Ctrl Pts',(84.569803483592,3.19667661862605,-3.07388273043659));
#20202=CARTESIAN_POINT('Ctrl Pts',(84.5640922713649,3.10747515059021,-3.16404561091582));
#20203=CARTESIAN_POINT('Ctrl Pts',(84.5583810591379,3.0144485895958,-3.2503213226824));
#20204=CARTESIAN_POINT('Ctrl Pts',(84.5526768134514,2.92153550246336,-3.33649179527748));
#20205=CARTESIAN_POINT('Ctrl Pts',(84.546972567765,2.82480689515587,-3.41878426333201));
#20206=CARTESIAN_POINT('Ctrl Pts',(84.5412683220785,2.72462086789934,-3.49684573954978));
#20207=CARTESIAN_POINT('Ctrl Pts',(84.5355696156728,2.62453212932434,-3.57483141180259));
#20208=CARTESIAN_POINT('Ctrl Pts',(84.5298709092672,2.52099296469723,-3.64859402386817));
#20209=CARTESIAN_POINT('Ctrl Pts',(84.5241722028615,2.41439660703346,-3.71781898751745));
#20210=CARTESIAN_POINT('Ctrl Pts',(84.5184776134606,2.30787725942763,-3.7869939399039));
#20211=CARTESIAN_POINT('Ctrl Pts',(84.5127830240597,2.19830544829266,-3.85163755184132));
#20212=CARTESIAN_POINT('Ctrl Pts',(84.5070884346589,2.08610522654049,-3.91147721248641));
#20213=CARTESIAN_POINT('Ctrl Pts',(84.5013959777942,1.97394702204781,-3.97129446409781));
#20214=CARTESIAN_POINT('Ctrl Pts',(84.4957035209296,1.85916271567687,-4.02631115391453));
#20215=CARTESIAN_POINT('Ctrl Pts',(84.4900110640649,1.74220263664386,-4.07629966671627));
#20216=CARTESIAN_POINT('Ctrl Pts',(84.4843195385025,1.62526169261295,-4.12628000125492));
#20217=CARTESIAN_POINT('Ctrl Pts',(84.47862801294,1.50614605086188,-4.17123363823749));
#20218=CARTESIAN_POINT('Ctrl Pts',(84.4729364873775,1.38532728884591,-4.21098056309678));
#20219=CARTESIAN_POINT('Ctrl Pts',(84.467244611106,1.26450108203617,-4.25072993714237));
#20220=CARTESIAN_POINT('Ctrl Pts',(84.4615527348344,1.14197192541054,-4.28527183621726));
#20221=CARTESIAN_POINT('Ctrl Pts',(84.4558608585629,1.01822737694168,-4.31447586722263));
#20222=CARTESIAN_POINT('Ctrl Pts',(84.450167349634,0.89444733359516,-4.34368827511022));
#20223=CARTESIAN_POINT('Ctrl Pts',(84.444473840705,0.76945159319912,-4.36755967736608));
#20224=CARTESIAN_POINT('Ctrl Pts',(84.4387803317761,0.643738234916988,-4.38601072558036));
#20225=CARTESIAN_POINT('Ctrl Pts',(84.4330807697288,0.517891223056601,-4.40448139023517));
#20226=CARTESIAN_POINT('Ctrl Pts',(84.4273812076814,0.391325465276577,-4.41752013693667));
#20227=CARTESIAN_POINT('Ctrl Pts',(84.4216816456341,0.264544811393503,-4.42509943874313));
#20228=CARTESIAN_POINT('Ctrl Pts',(84.4159786311388,0.137687361502868,-4.43268333162955));
#20229=CARTESIAN_POINT('Ctrl Pts',(84.4102756166435,0.0106151546344382,
-4.43480118504154));
#20230=CARTESIAN_POINT('Ctrl Pts',(84.4045726021483,-0.116168859317712,
-4.43147760866788));
#20231=CARTESIAN_POINT('Ctrl Pts',(84.398861420238,-0.243134443500064,-4.42814927252596));
#20232=CARTESIAN_POINT('Ctrl Pts',(84.3931502383277,-0.369810613339101,
-4.41936397378047));
#20233=CARTESIAN_POINT('Ctrl Pts',(84.3874390564175,-0.49570005297812,-4.4051981178464));
#20234=CARTESIAN_POINT('Ctrl Pts',(84.3849366491739,-0.550859676782646,
-4.39899121688288));
#20235=CARTESIAN_POINT('Ctrl Pts',(84.3824342419302,-0.605868397615598,
-4.39175199917643));
#20236=CARTESIAN_POINT('Ctrl Pts',(84.3799318346866,-0.660685147178269,
-4.38348994937801));
#20237=CARTESIAN_POINT('Ctrl Pts',(84.3742207423032,-0.785790092308468,
-4.3646339738789));
#20238=CARTESIAN_POINT('Ctrl Pts',(84.3685096499199,-0.910280175299019,
-4.34038890063126));
#20239=CARTESIAN_POINT('Ctrl Pts',(84.3627985575365,-1.03365613806391,-4.31080549181273));
#20240=CARTESIAN_POINT('Ctrl Pts',(84.3570944317305,-1.15688160279174,-4.28125816980444));
#20241=CARTESIAN_POINT('Ctrl Pts',(84.3513903059246,-1.27899526623601,-4.24638555975464));
#20242=CARTESIAN_POINT('Ctrl Pts',(84.3456861801186,-1.39950483410601,-4.20628995901541));
#20243=CARTESIAN_POINT('Ctrl Pts',(84.3399875934903,-1.51989737722392,-4.16623329441893));
#20244=CARTESIAN_POINT('Ctrl Pts',(84.3342890068621,-1.63868854776384,-4.1209638569014));
#20245=CARTESIAN_POINT('Ctrl Pts',(84.3285904202338,-1.75539852810498,-4.07063447235525));
#20246=CARTESIAN_POINT('Ctrl Pts',(84.3228959503677,-1.87202419504252,-4.02034144666803));
#20247=CARTESIAN_POINT('Ctrl Pts',(84.3172014805016,-1.98657129888928,-3.96499590682139));
#20248=CARTESIAN_POINT('Ctrl Pts',(84.3115070106355,-2.09857786815734,-3.90479960193608));
#20249=CARTESIAN_POINT('Ctrl Pts',(84.3058146725113,-2.21054250742934,-3.84462583171854));
#20250=CARTESIAN_POINT('Ctrl Pts',(84.3001223343871,-2.31996815210041,-3.7796050957292));
#20251=CARTESIAN_POINT('Ctrl Pts',(84.2944299962629,-2.4264157079711,-3.70998595847897));
#20252=CARTESIAN_POINT('Ctrl Pts',(84.2887385889112,-2.53284585826152,-3.64037820487651));
#20253=CARTESIAN_POINT('Ctrl Pts',(84.2830471815594,-2.63629855440457,-3.56617376401281));
#20254=CARTESIAN_POINT('Ctrl Pts',(84.2773557742077,-2.73636253555055,-3.48766527551532));
#20255=CARTESIAN_POINT('Ctrl Pts',(84.2716640154919,-2.83643269423456,-3.40915194022712));
#20256=CARTESIAN_POINT('Ctrl Pts',(84.265972256776,-2.93311340777536,-3.32633427523276));
#20257=CARTESIAN_POINT('Ctrl Pts',(84.2602804980602,-3.02602585128815,-3.23954573163211));
#20258=CARTESIAN_POINT('Ctrl Pts',(84.2545871059062,-3.11896495909711,-3.15273228119075));
#20259=CARTESIAN_POINT('Ctrl Pts',(84.2488937137521,-3.20813335395086,-3.06194595750582));
#20260=CARTESIAN_POINT('Ctrl Pts',(84.243200321598,-3.29318885840884,-2.96755726867265));
#20261=CARTESIAN_POINT('Ctrl Pts',(84.2375008745215,-3.37833481939359,-2.87306819747137));
#20262=CARTESIAN_POINT('Ctrl Pts',(84.231801427445,-3.45935888923631,-2.77496940867005));
#20263=CARTESIAN_POINT('Ctrl Pts',(84.2261019803686,-3.53595881828426,-2.67366494449057));
#20264=CARTESIAN_POINT('Ctrl Pts',(84.2203990799687,-3.61260515961086,-2.57229909943154));
#20265=CARTESIAN_POINT('Ctrl Pts',(84.2146961795688,-3.68482179360344,-2.46772403755889));
#20266=CARTESIAN_POINT('Ctrl Pts',(84.208993279169,-3.75235035936997,-2.36037195808967));
#20267=CARTESIAN_POINT('Ctrl Pts',(84.2032822090281,-3.81997566378722,-2.25286609043907));
#20268=CARTESIAN_POINT('Ctrl Pts',(84.1975711388873,-3.88289929247917,-2.14257560752219));
#20269=CARTESIAN_POINT('Ctrl Pts',(84.1918600687465,-3.94090911427975,-2.02995673672785));
#20270=CARTESIAN_POINT('Ctrl Pts',(84.1893563703491,-3.96634026716265,-1.98058530906659));
#20271=CARTESIAN_POINT('Ctrl Pts',(84.1868526719517,-3.99082766603068,-1.93076664398898));
#20272=CARTESIAN_POINT('Ctrl Pts',(84.1843489735543,-4.01435641213992,-1.88054024054554));
#20273=CARTESIAN_POINT('Ctrl Pts',(84.1781915115531,-4.07222175257094,-1.75701610881383));
#20274=CARTESIAN_POINT('Ctrl Pts',(84.1720340495519,-4.1244421435033,-1.63069055220892));
#20275=CARTESIAN_POINT('Ctrl Pts',(84.1658765875508,-4.17076017586692,-1.50208140771481));
#20276=CARTESIAN_POINT('Ctrl Pts',(84.1597384307519,-4.21693298947263,-1.37387548544901));
#20277=CARTESIAN_POINT('Ctrl Pts',(84.153600273953,-4.25724025001845,-1.24340053497881));
#20278=CARTESIAN_POINT('Ctrl Pts',(84.1474621171541,-4.29147259395242,-1.11119394137804));
#20279=CARTESIAN_POINT('Ctrl Pts',(84.1413358900107,-4.3256384065015,-0.979244294476043));
#20280=CARTESIAN_POINT('Ctrl Pts',(84.1352096628674,-4.35375275848106,-0.845569999491432));
#20281=CARTESIAN_POINT('Ctrl Pts',(84.1290834357241,-4.37565515223945,-0.710725677515822));
#20282=CARTESIAN_POINT('Ctrl Pts',(84.1229755449203,-4.39749199019677,-0.576284956518449));
#20283=CARTESIAN_POINT('Ctrl Pts',(84.1168676541165,-4.41315389735394,-0.440681485826579));
#20284=CARTESIAN_POINT('Ctrl Pts',(84.1107597633126,-4.42253098370653,-0.304481030863648));
#20285=CARTESIAN_POINT('Ctrl Pts',(84.1062374819958,-4.42947377685407,-0.203638237073225));
#20286=CARTESIAN_POINT('Ctrl Pts',(84.101715200679,-4.43297229034197,-0.102468536838374));
#20287=CARTESIAN_POINT('Ctrl Pts',(84.0971929193621,-4.43299983598826,-0.00120587233263017));
#20288=CARTESIAN_POINT('Ctrl Pts',(84.0971929193385,-4.4329998359884,-0.00120587180341138));
#20289=CARTESIAN_POINT('Ctrl Pts',(84.0913529328301,-4.43303540788692,0.12956277196029));
#20290=CARTESIAN_POINT('Ctrl Pts',(84.0855129463217,-4.42728033452424,0.26028024094117));
#20291=CARTESIAN_POINT('Ctrl Pts',(84.0796729598133,-4.415774401046,0.390417006631218));
#20292=CARTESIAN_POINT('Ctrl Pts',(84.0738291793772,-4.40426099277658,0.5206383152355));
#20293=CARTESIAN_POINT('Ctrl Pts',(84.0679853989411,-4.38698931100753,0.650277801680128));
#20294=CARTESIAN_POINT('Ctrl Pts',(84.062141618505,-4.36405081751758,0.778812854365017));
#20295=CARTESIAN_POINT('Ctrl Pts',(84.0560269929981,-4.34004918040645,0.913305195457647));
#20296=CARTESIAN_POINT('Ctrl Pts',(84.0499123674912,-4.30984296405206,1.04658782571554));
#20297=CARTESIAN_POINT('Ctrl Pts',(84.0437977419842,-4.2735958871232,1.17807775361548));
#20298=CARTESIAN_POINT('Ctrl Pts',(84.0379393301313,-4.23886762700767,1.30405802031789));
#20299=CARTESIAN_POINT('Ctrl Pts',(84.0320809182784,-4.1985946681494,1.42839244942262));
#20300=CARTESIAN_POINT('Ctrl Pts',(84.0262225064255,-4.15297088683791,1.55058757027029));
#20301=CARTESIAN_POINT('Ctrl Pts',(84.0203584203072,-4.10730291582958,1.67290104530059));
#20302=CARTESIAN_POINT('Ctrl Pts',(84.0144943341889,-4.05627393146945,1.79307074206799));
#20303=CARTESIAN_POINT('Ctrl Pts',(84.0086302480705,-4.00012480179417,1.91062570119612));
#20304=CARTESIAN_POINT('Ctrl Pts',(84.0027563569163,-3.94388178805554,2.02837721790747));
#20305=CARTESIAN_POINT('Ctrl Pts',(83.9968824657621,-3.88250170262343,2.14350494074438));
#20306=CARTESIAN_POINT('Ctrl Pts',(83.9910085746079,-3.81627026328809,2.25556429248715));
#20307=CARTESIAN_POINT('Ctrl Pts',(83.9902610872125,-3.80784192085246,2.26982450786342));
#20308=CARTESIAN_POINT('Ctrl Pts',(83.9895135998172,-3.79933507053889,2.28403507546932));
#20309=CARTESIAN_POINT('Ctrl Pts',(83.9887661124219,-3.7907503488902,2.29819511625728));
#20310=CARTESIAN_POINT('Ctrl Pts',(83.983054636412,-3.7251553541719,2.4063905637869));
#20311=CARTESIAN_POINT('Ctrl Pts',(83.9773431604021,-3.65482340222278,2.51194223722398));
#20312=CARTESIAN_POINT('Ctrl Pts',(83.9716316843921,-3.57999371167098,2.61440892447915));
#20313=CARTESIAN_POINT('Ctrl Pts',(83.965927173822,-3.50525527978894,2.71675064832067));
#20314=CARTESIAN_POINT('Ctrl Pts',(83.9602226632518,-3.42603025544912,2.81601455147138));
#20315=CARTESIAN_POINT('Ctrl Pts',(83.9545181526817,-3.34260273108345,2.91178570333626));
#20316=CARTESIAN_POINT('Ctrl Pts',(83.9488191806154,-3.25925620642181,3.00746387108092));
#20317=CARTESIAN_POINT('Ctrl Pts',(83.9431202085492,-3.17171556145002,3.09965573613323));
#20318=CARTESIAN_POINT('Ctrl Pts',(83.9374212364829,-3.08030670995789,3.18797734819249));
#20319=CARTESIAN_POINT('Ctrl Pts',(83.9317263809658,-2.98896388599269,3.27623516273625));
#20320=CARTESIAN_POINT('Ctrl Pts',(83.9260315254487,-2.8937587027215,3.36062801202631));
#20321=CARTESIAN_POINT('Ctrl Pts',(83.9203366699316,-2.79505534578238,3.44080726196823));
#20322=CARTESIAN_POINT('Ctrl Pts',(83.9146439472549,-2.69638895527797,3.52095648313404));
#20323=CARTESIAN_POINT('Ctrl Pts',(83.9089512245782,-2.59422730538682,3.59689499148059));
#20324=CARTESIAN_POINT('Ctrl Pts',(83.9032585019015,-2.48896897063816,3.66831329948799));
#20325=CARTESIAN_POINT('Ctrl Pts',(83.8975667107976,-2.38372786065409,3.73971992040622));
#20326=CARTESIAN_POINT('Ctrl Pts',(83.8918749196937,-2.27539140392943,3.80660758831022));
#20327=CARTESIAN_POINT('Ctrl Pts',(83.8861831285899,-2.16438812667184,3.86870947954508));
#20328=CARTESIAN_POINT('Ctrl Pts',(83.8804909873342,-2.05337802063171,3.93081519121048));
#20329=CARTESIAN_POINT('Ctrl Pts',(83.8747988460785,-1.93970111607934,3.98813434577702));
#20330=CARTESIAN_POINT('Ctrl Pts',(83.8691067048227,-1.82381110683975,4.04044577324928));
#20331=CARTESIAN_POINT('Ctrl Pts',(83.8634129317538,-1.70788787445219,4.09277219727134));
#20332=CARTESIAN_POINT('Ctrl Pts',(83.8577191586848,-1.58975063885866,4.14008787413932));
#20333=CARTESIAN_POINT('Ctrl Pts',(83.8520253856159,-1.46987317524154,4.18221972745399));
#20334=CARTESIAN_POINT('Ctrl Pts',(83.8463255621315,-1.34986832536405,4.22439635164614));
#20335=CARTESIAN_POINT('Ctrl Pts',(83.840625738647,-1.22811993212665,4.26137802144207));
#20336=CARTESIAN_POINT('Ctrl Pts',(83.8349259151626,-1.10511733767614,4.2930414242082));
#20337=CARTESIAN_POINT('Ctrl Pts',(83.829222640422,-0.982040264870982,4.32472399923774));
#20338=CARTESIAN_POINT('Ctrl Pts',(83.8235193656813,-0.857707867782099,
4.35108180951428));
#20339=CARTESIAN_POINT('Ctrl Pts',(83.8178160909406,-0.732618569098261,
4.37204289002434));
#20340=CARTESIAN_POINT('Ctrl Pts',(83.8121046528678,-0.607350224946806,
4.39303397299266));
#20341=CARTESIAN_POINT('Ctrl Pts',(83.806393214795,-0.481323211148197,4.40861285320017));
#20342=CARTESIAN_POINT('Ctrl Pts',(83.8006817767222,-0.35504031884819,4.41875948338356));
#20343=CARTESIAN_POINT('Ctrl Pts',(83.7981822682446,-0.29977487504039,4.42319997417393));
#20344=CARTESIAN_POINT('Ctrl Pts',(83.795682759767,-0.244460417594769,4.42660074476098));
#20345=CARTESIAN_POINT('Ctrl Pts',(83.7931832512895,-0.189138922143068,
4.42896324980582));
#20346=CARTESIAN_POINT('Ctrl Pts',(83.7874728176785,-0.0627501821680352,
4.43436068227514));
#20347=CARTESIAN_POINT('Ctrl Pts',(83.7817623840675,0.0640650031860301,
4.43435204042131));
#20348=CARTESIAN_POINT('Ctrl Pts',(83.7760519504566,0.190806976161237,4.42889170084889));
#20349=CARTESIAN_POINT('Ctrl Pts',(83.7703484833763,0.317394328331168,4.42343802270111));
#20350=CARTESIAN_POINT('Ctrl Pts',(83.764645016296,0.443908250334559,4.41254589560693));
#20351=CARTESIAN_POINT('Ctrl Pts',(83.7589415492157,0.569846065609721,4.39622161196511));
#20352=CARTESIAN_POINT('Ctrl Pts',(83.7532436205021,0.695661588640037,4.3799131800616));
#20353=CARTESIAN_POINT('Ctrl Pts',(83.7475456917884,0.820901724396628,4.35818313890482));
#20354=CARTESIAN_POINT('Ctrl Pts',(83.7418477630747,0.945066382485209,4.33108976271519));
#20355=CARTESIAN_POINT('Ctrl Pts',(83.736153949551,1.06914136568023,4.30401595405519));
#20356=CARTESIAN_POINT('Ctrl Pts',(83.7304601360273,1.19214202838096,4.27158660466542));
#20357=CARTESIAN_POINT('Ctrl Pts',(83.7247663225036,1.31357644502133,4.23391142126109));
#20358=CARTESIAN_POINT('Ctrl Pts',(83.7190746360093,1.43496549758774,4.19625031211885));
#20359=CARTESIAN_POINT('Ctrl Pts',(83.713382949515,1.55478908672782,4.15334738351648));
#20360=CARTESIAN_POINT('Ctrl Pts',(83.7076912630207,1.67256879373474,4.10536266731999));
#20361=CARTESIAN_POINT('Ctrl Pts',(83.7020005041744,1.79032930465516,4.05738577181509));
#20362=CARTESIAN_POINT('Ctrl Pts',(83.696309745328,1.90604622640667,4.00432888674341));
#20363=CARTESIAN_POINT('Ctrl Pts',(83.6906189864817,2.01926003747436,3.94640062602101));
#20364=CARTESIAN_POINT('Ctrl Pts',(83.684927872462,2.13248091447746,3.88846874986208));
#20365=CARTESIAN_POINT('Ctrl Pts',(83.6792367584422,2.24319801462135,3.82566507523673));
#20366=CARTESIAN_POINT('Ctrl Pts',(83.6735456444225,2.35097585630249,3.75824447356512));
#20367=CARTESIAN_POINT('Ctrl Pts',(83.6678528924675,2.45878471706596,3.69080446785683));
#20368=CARTESIAN_POINT('Ctrl Pts',(83.6621601405124,2.56365229815003,3.61874510337618));
#20369=CARTESIAN_POINT('Ctrl Pts',(83.6564673885573,2.66517201029379,3.54236462769526));
#20370=CARTESIAN_POINT('Ctrl Pts',(83.6507685714675,2.76679988290871,3.46590277522492));
#20371=CARTESIAN_POINT('Ctrl Pts',(83.6450697543777,2.86507244561426,3.3851108598858));
#20372=CARTESIAN_POINT('Ctrl Pts',(83.6393709372879,2.95961589459052,3.30032767410861));
#20373=CARTESIAN_POINT('Ctrl Pts',(83.6336686618933,3.05421671688846,3.21549303798723));
#20374=CARTESIAN_POINT('Ctrl Pts',(83.6279663864987,3.14508363230125,3.12666258503787));
#20375=CARTESIAN_POINT('Ctrl Pts',(83.622264111104,3.23188053981087,3.0342111291721));
#20376=CARTESIAN_POINT('Ctrl Pts',(83.6165536529411,3.31880200093002,2.94162700541682));
#20377=CARTESIAN_POINT('Ctrl Pts',(83.6108431947782,3.4016415322164,2.84541180519697));
#20378=CARTESIAN_POINT('Ctrl Pts',(83.6051327366153,3.4801038216176,2.74597275856164));
#20379=CARTESIAN_POINT('Ctrl Pts',(83.6026219544625,3.51460222967349,2.70225126083712));
#20380=CARTESIAN_POINT('Ctrl Pts',(83.6001111723098,3.54825499981515,2.65790690039704));
#20381=CARTESIAN_POINT('Ctrl Pts',(83.5976003901571,3.5810397745534,2.61297591513327));
#20382=CARTESIAN_POINT('Ctrl Pts',(83.5918888133932,3.65561922677717,2.51076602363333));
#20383=CARTESIAN_POINT('Ctrl Pts',(83.5861772366293,3.72593433224448,2.40520296959203));
#20384=CARTESIAN_POINT('Ctrl Pts',(83.5804656598655,3.79167004282015,2.29667744500186));
#20385=CARTESIAN_POINT('Ctrl Pts',(83.574761055143,3.85732551073857,2.188284395993));
#20386=CARTESIAN_POINT('Ctrl Pts',(83.5690564504205,3.91841250000079,2.07693640934517));
#20387=CARTESIAN_POINT('Ctrl Pts',(83.5633518456981,3.97465749836092,1.96305546807096));
#20388=CARTESIAN_POINT('Ctrl Pts',(83.5576527860998,4.03084782413389,1.84928522402975));
#20389=CARTESIAN_POINT('Ctrl Pts',(83.5519537265015,4.0822053488005,1.73298728050214));
#20390=CARTESIAN_POINT('Ctrl Pts',(83.5462546669032,4.12850125681246,1.61461028502172));
#20391=CARTESIAN_POINT('Ctrl Pts',(83.5405597304986,4.17476367035164,1.49631893372075));
#20392=CARTESIAN_POINT('Ctrl Pts',(83.534864794094,4.21597161089721,1.37595189463706));
#20393=CARTESIAN_POINT('Ctrl Pts',(83.5291698576894,4.25194359409921,1.25397953436198));
#20394=CARTESIAN_POINT('Ctrl Pts',(83.5234770641988,4.28790204161613,1.13205307034589));
#20395=CARTESIAN_POINT('Ctrl Pts',(83.5177842707082,4.31862833657742,1.00852286840435));
#20396=CARTESIAN_POINT('Ctrl Pts',(83.5120914772176,4.34399036560862,0.88387595481463));
#20397=CARTESIAN_POINT('Ctrl Pts',(83.5063996215779,4.36934821640941,0.759249575998512));
#20398=CARTESIAN_POINT('Ctrl Pts',(83.5007077659382,4.3893434795575,0.633507242415827));
#20399=CARTESIAN_POINT('Ctrl Pts',(83.4950159102986,4.40389494948329,0.507147191568224));
#20400=CARTESIAN_POINT('Ctrl Pts',(83.4893237108232,4.41844729843957,0.380779507516781));
#20401=CARTESIAN_POINT('Ctrl Pts',(83.4836315113479,4.42755515447289,0.253794428480396));
#20402=CARTESIAN_POINT('Ctrl Pts',(83.4779393118725,4.43118913666873,0.126695836825879));
#20403=CARTESIAN_POINT('Ctrl Pts',(83.4722454869427,4.43482415657815,-0.000439048879321308));
#20404=CARTESIAN_POINT('Ctrl Pts',(83.4665516620128,4.43298218168202,-0.127687112904415));
#20405=CARTESIAN_POINT('Ctrl Pts',(83.460857837083,4.42568594876661,-0.254544461518653));
#20406=CARTESIAN_POINT('Ctrl Pts',(83.4551579715224,4.41838197521124,-0.381536394249353));
#20407=CARTESIAN_POINT('Ctrl Pts',(83.4494581059619,4.40561221322122,-0.508136385150158));
#20408=CARTESIAN_POINT('Ctrl Pts',(83.4437582404013,4.38745132005257,-0.633845339313109));
#20409=CARTESIAN_POINT('Ctrl Pts',(83.438054929118,4.36927944813329,-0.759630287935535));
#20410=CARTESIAN_POINT('Ctrl Pts',(83.4323516178347,4.34571002640231,-0.884522735206173));
#20411=CARTESIAN_POINT('Ctrl Pts',(83.4266483065514,4.31686859648169,-1.00803497990406));
#20412=CARTESIAN_POINT('Ctrl Pts',(83.4209368406541,4.28798592898571,-1.13172382283282));
#20413=CARTESIAN_POINT('Ctrl Pts',(83.4152253747567,4.25381630894877,-1.25402813920103));
#20414=CARTESIAN_POINT('Ctrl Pts',(83.4095139088594,4.21453487374948,-1.37447619039017));
#20415=CARTESIAN_POINT('Ctrl Pts',(83.4070151155812,4.19734906051016,-1.4271727810894));
#20416=CARTESIAN_POINT('Ctrl Pts',(83.404516322303,4.17918541196736,-1.4795143296501));
#20417=CARTESIAN_POINT('Ctrl Pts',(83.4020175290248,4.16006142107037,-1.53146269067254));
#20418=CARTESIAN_POINT('Ctrl Pts',(83.3963041942983,4.11633561059467,-1.65023937284239));
#20419=CARTESIAN_POINT('Ctrl Pts',(83.3905908595718,4.06745177772856,-1.76732409392234));
#20420=CARTESIAN_POINT('Ctrl Pts',(83.3848775248453,4.01356072289606,-1.88223784990793));
#20421=CARTESIAN_POINT('Ctrl Pts',(83.3791711450774,3.959735270741,-1.9970117190405));
#20422=CARTESIAN_POINT('Ctrl Pts',(83.3734647653095,3.90091489140313,-2.10961952289275));
#20423=CARTESIAN_POINT('Ctrl Pts',(83.3677583855417,3.83729944594922,-2.21959950489222));
#20424=CARTESIAN_POINT('Ctrl Pts',(83.3620575361312,3.7737456536217,-2.32947289941625));
#20425=CARTESIAN_POINT('Ctrl Pts',(83.3563566867208,3.70540624107761,-2.43672319658693));
#20426=CARTESIAN_POINT('Ctrl Pts',(83.3506558373104,3.6325280306422,-2.54091107805817));
#20427=CARTESIAN_POINT('Ctrl Pts',(83.344959098619,3.55970237059481,-2.64502383263528));
#20428=CARTESIAN_POINT('Ctrl Pts',(83.3392623599276,3.48234465443669,-2.74607824093065));
#20429=CARTESIAN_POINT('Ctrl Pts',(83.3335656212362,3.40074601005896,-2.84366235250743));
#20430=CARTESIAN_POINT('Ctrl Pts',(83.3278710137284,3.31917789221498,-2.94120995729297));
#20431=CARTESIAN_POINT('Ctrl Pts',(83.3221764062205,3.23337225624653,-3.03528954135123));
#20432=CARTESIAN_POINT('Ctrl Pts',(83.3164817987127,3.14366145661774,-3.12552101995427));
#20433=CARTESIAN_POINT('Ctrl Pts',(83.3107881223432,3.05396532580863,-3.21573774460022));
#20434=CARTESIAN_POINT('Ctrl Pts',(83.3050944459738,2.960365582564,-3.30210733266954));
#20435=CARTESIAN_POINT('Ctrl Pts',(83.2994007696043,2.8632321262774,-3.38428586130856));
#20436=CARTESIAN_POINT('Ctrl Pts',(83.2937067447069,2.76609272414436,-3.46646942035554));
#20437=CARTESIAN_POINT('Ctrl Pts',(83.2880127198095,2.66541948321974,-3.54446115213014));
#20438=CARTESIAN_POINT('Ctrl Pts',(83.282318694912,2.5616157255802,-3.617957141048));
#20439=CARTESIAN_POINT('Ctrl Pts',(83.2766230418857,2.45778228666819,-3.69147414514414));
#20440=CARTESIAN_POINT('Ctrl Pts',(83.2709273888593,2.35081687564506,-3.76049261868623));
#20441=CARTESIAN_POINT('Ctrl Pts',(83.2652317358329,2.24115171398086,-3.82475201744122));
#20442=CARTESIAN_POINT('Ctrl Pts',(83.2595300481698,2.13137036029987,-3.88907950007103));
#20443=CARTESIAN_POINT('Ctrl Pts',(83.2538283605067,2.01888388917474,-3.94863763852377));
#20444=CARTESIAN_POINT('Ctrl Pts',(83.2481266728436,1.90414931067986,-4.00321176090366));
#20445=CARTESIAN_POINT('Ctrl Pts',(83.2424215404412,1.7893454139882,-4.0578188548585));
#20446=CARTESIAN_POINT('Ctrl Pts',(83.2367164080389,1.67229107071298,-4.10743577863478));
#20447=CARTESIAN_POINT('Ctrl Pts',(83.2310112756365,1.5534620216424,-4.15189652415793));
#20448=CARTESIAN_POINT('Ctrl Pts',(83.22529800601,1.43446348682922,-4.19642068399374));
#20449=CARTESIAN_POINT('Ctrl Pts',(83.2195847363836,1.31368557021128,-4.23577385751035));
#20450=CARTESIAN_POINT('Ctrl Pts',(83.2138714667571,1.19161822687623,-4.26984016110397));
#20451=CARTESIAN_POINT('Ctrl Pts',(83.2113925338022,1.13865437607026,-4.28462120386076));
#20452=CARTESIAN_POINT('Ctrl Pts',(83.2089136008473,1.08544789663886,-4.29840759029817));
#20453=CARTESIAN_POINT('Ctrl Pts',(83.2064346678924,1.03203923524623,-4.31119287632928));
#20454=CARTESIAN_POINT('Ctrl Pts',(83.2007300562091,0.90913325944449,-4.34061484674728));
#20455=CARTESIAN_POINT('Ctrl Pts',(83.1950254445258,0.784776113443813,-4.36482277943889));
#20456=CARTESIAN_POINT('Ctrl Pts',(83.1893208328425,0.659448564409288,-4.38367615032161));
#20457=CARTESIAN_POINT('Ctrl Pts',(83.1836231915243,0.534274150910706,-4.40250648460084));
#20458=CARTESIAN_POINT('Ctrl Pts',(83.177925550206,0.408132085508736,-4.41599521387896));
#20459=CARTESIAN_POINT('Ctrl Pts',(83.1722279088878,0.281516077405062,-4.42405218076849));
#20460=CARTESIAN_POINT('Ctrl Pts',(83.1665358030648,0.155023082012252,-4.43210131998005));
#20461=CARTESIAN_POINT('Ctrl Pts',(83.1608436972417,0.0280574572038139,
-4.43472917186113));
#20462=CARTESIAN_POINT('Ctrl Pts',(83.1551515914187,-0.0988796452240617,
-4.43189708993343));
#20463=CARTESIAN_POINT('Ctrl Pts',(83.1494635912445,-0.225725189414087,
-4.42906705075308));
#20464=CARTESIAN_POINT('Ctrl Pts',(83.1437755910704,-0.352541853464863,
-4.4207849244752));
#20465=CARTESIAN_POINT('Ctrl Pts',(83.1380875908963,-0.478826635252343,
-4.40706410815329));
#20466=CARTESIAN_POINT('Ctrl Pts',(83.1324016826762,-0.605064971550271,
-4.39334833812454));
#20467=CARTESIAN_POINT('Ctrl Pts',(83.126715774456,-0.730771417290483,-4.3741978978697));
#20468=CARTESIAN_POINT('Ctrl Pts',(83.1210298662359,-0.855446582372364,
-4.34967816564714));
#20469=CARTESIAN_POINT('Ctrl Pts',(83.1153448622648,-0.980101919944643,
-4.32516233287981));
#20470=CARTESIAN_POINT('Ctrl Pts',(83.1096598582938,-1.10372591053141,-4.29527898367961));
#20471=CARTESIAN_POINT('Ctrl Pts',(83.1039748543227,-1.22582841724243,-4.26014479700877));
#20472=CARTESIAN_POINT('Ctrl Pts',(83.0982894657907,-1.34793918355144,-4.22500823369338));
#20473=CARTESIAN_POINT('Ctrl Pts',(83.0926040772588,-1.46852787668371,-4.18462023711314));
#20474=CARTESIAN_POINT('Ctrl Pts',(83.0869186887268,-1.58711911719866,-4.13914748563307));
#20475=CARTESIAN_POINT('Ctrl Pts',(83.0812316268597,-1.70574526172996,-4.09366135051981));
#20476=CARTESIAN_POINT('Ctrl Pts',(83.0755445649925,-1.82237241065795,-4.04308762666087));
#20477=CARTESIAN_POINT('Ctrl Pts',(83.0698575031254,-1.93654526686745,-3.98764108582672));
#20478=CARTESIAN_POINT('Ctrl Pts',(83.0641642922638,-2.05084156964352,-3.93213459479668));
#20479=CARTESIAN_POINT('Ctrl Pts',(83.0584710814022,-2.16267792118752,-3.87174494253703));
#20480=CARTESIAN_POINT('Ctrl Pts',(83.0527778705406,-2.27162347021219,-3.8067329574822));
#20481=CARTESIAN_POINT('Ctrl Pts',(83.0470811612202,-2.38063596590833,-3.74168102278238));
#20482=CARTESIAN_POINT('Ctrl Pts',(83.0413844518998,-2.48675378667198,-3.67200131658452));
#20483=CARTESIAN_POINT('Ctrl Pts',(83.0356877425793,-2.58957623773381,-3.59799720802621));
#20484=CARTESIAN_POINT('Ctrl Pts',(83.0299827406343,-2.69254836608165,-3.52388537266302));
#20485=CARTESIAN_POINT('Ctrl Pts',(83.0242777386892,-2.79221523266356,-3.4454368125276));
#20486=CARTESIAN_POINT('Ctrl Pts',(83.0185727367441,-2.88821001233549,-3.36299448775121));
#20487=CARTESIAN_POINT('Ctrl Pts',(83.0159990934161,-2.9315152253059,-3.3258030650049));
#20488=CARTESIAN_POINT('Ctrl Pts',(83.0134254500881,-2.97407364034082,-3.28779936335854));
#20489=CARTESIAN_POINT('Ctrl Pts',(83.0108518067601,-3.01585417860915,-3.24901717037102));
#20490=CARTESIAN_POINT('Ctrl Pts',(83.0052145989932,-3.10736863683513,-3.16407017047183));
#20491=CARTESIAN_POINT('Ctrl Pts',(82.9995773912263,-3.19545120876946,-3.07510492987072));
#20492=CARTESIAN_POINT('Ctrl Pts',(82.9939401834594,-3.2797227815974,-2.982433146924));
#20493=CARTESIAN_POINT('Ctrl Pts',(82.988309963474,-3.36388989289898,-2.88987623825306));
#20494=CARTESIAN_POINT('Ctrl Pts',(82.9826797434884,-3.4442551250556,-2.79362222478303));
#20495=CARTESIAN_POINT('Ctrl Pts',(82.977049523503,-3.52047370683076,-2.69402187806879));
#20496=CARTESIAN_POINT('Ctrl Pts',(82.9714254739873,-3.59660875644143,-2.59453068889005));
#20497=CARTESIAN_POINT('Ctrl Pts',(82.9658014244717,-3.66860595187104,-2.49170078963833));
#20498=CARTESIAN_POINT('Ctrl Pts',(82.9601773749561,-3.73615911197191,-2.38591787160189));
#20499=CARTESIAN_POINT('Ctrl Pts',(82.9545567511598,-3.80367112411159,-2.28019938802564));
#20500=CARTESIAN_POINT('Ctrl Pts',(82.9489361273636,-3.86674426160977,-2.17153180635648));
#20501=CARTESIAN_POINT('Ctrl Pts',(82.9433155035674,-3.92511438630353,-2.06033153993066));
#20502=CARTESIAN_POINT('Ctrl Pts',(82.9376969531584,-3.9834629788903,-1.9491722940791));
#20503=CARTESIAN_POINT('Ctrl Pts',(82.9320784027494,-4.03711181792837,-1.83548258460658));
#20504=CARTESIAN_POINT('Ctrl Pts',(82.9264598523405,-4.08584198861877,-1.71970469675459));
#20505=CARTESIAN_POINT('Ctrl Pts',(82.9208420249266,-4.13456588871013,-1.60394170720281));
#20506=CARTESIAN_POINT('Ctrl Pts',(82.9152241975128,-4.17837222128289,-1.48609145278783));
#20507=CARTESIAN_POINT('Ctrl Pts',(82.909606370099,-4.21708990039573,-1.36661690754224));
#20508=CARTESIAN_POINT('Ctrl Pts',(82.9039855488592,-4.25582821275085,-1.24707869248756));
#20509=CARTESIAN_POINT('Ctrl Pts',(82.8983647276194,-4.28947232540022,-1.12591484803288));
#20510=CARTESIAN_POINT('Ctrl Pts',(82.8927439063795,-4.31790083432927,-1.00360419733011));
#20511=CARTESIAN_POINT('Ctrl Pts',(82.8871215575249,-4.34633706949776,-0.881260305299895));
#20512=CARTESIAN_POINT('Ctrl Pts',(82.8814992086703,-4.36955479795709,-0.757769389447973));
#20513=CARTESIAN_POINT('Ctrl Pts',(82.8758768598157,-4.38748390115548,-0.633619773287978));
#20514=CARTESIAN_POINT('Ctrl Pts',(82.8702483134227,-4.40543276767853,-0.509333306492264));
#20515=CARTESIAN_POINT('Ctrl Pts',(82.8646197670297,-4.41808132081018,-0.384387097784731));
#20516=CARTESIAN_POINT('Ctrl Pts',(82.8589912206366,-4.42541138808375,-0.259274075485084));
#20517=CARTESIAN_POINT('Ctrl Pts',(82.855058453546,-4.43053303856554,-0.171855345612122));
#20518=CARTESIAN_POINT('Ctrl Pts',(82.8511256864554,-4.43305926183473,-0.0843552441526603));
#20519=CARTESIAN_POINT('Ctrl Pts',(82.8471929193648,-4.43299894467431,0.00305884233548282));
#20520=CARTESIAN_POINT('Origin',(80.1322559480305,0.,0.));
#20521=CARTESIAN_POINT('',(89.5072559480779,-3.72274932293675,0.00224523361020461));
#20522=CARTESIAN_POINT('Ctrl Pts',(89.3502471949048,-2.62112000711957,2.64359555733806));
#20523=CARTESIAN_POINT('Ctrl Pts',(89.3561947378413,-2.70028756086394,2.5651010771752));
#20524=CARTESIAN_POINT('Ctrl Pts',(89.3621422807778,-2.77597243042016,2.48300129230493));
#20525=CARTESIAN_POINT('Ctrl Pts',(89.3680898237143,-2.84783768146393,2.39764219652019));
#20526=CARTESIAN_POINT('Ctrl Pts',(89.374035835165,-2.91968442728483,2.31230508060844));
#20527=CARTESIAN_POINT('Ctrl Pts',(89.3799818466158,-2.98771324183078,2.2237106411624));
#20528=CARTESIAN_POINT('Ctrl Pts',(89.3859278580665,-3.05162626314291,2.13223936568961));
#20529=CARTESIAN_POINT('Ctrl Pts',(89.3918737993332,-3.11553853005399,2.04076916990333));
#20530=CARTESIAN_POINT('Ctrl Pts',(89.3978197405998,-3.17533486192985,1.94642254760151));
#20531=CARTESIAN_POINT('Ctrl Pts',(89.4037656818665,-3.23076011931727,1.84960985451772));
#20532=CARTESIAN_POINT('Ctrl Pts',(89.4097130138169,-3.28619834000165,1.75277451811663));
#20533=CARTESIAN_POINT('Ctrl Pts',(89.4156603457672,-3.33726324673087,1.65347232600807));
#20534=CARTESIAN_POINT('Ctrl Pts',(89.4216076777176,-3.38374551156931,1.55213848461875));
#20535=CARTESIAN_POINT('Ctrl Pts',(89.4275612789431,-3.43027677486806,1.45069782394632));
#20536=CARTESIAN_POINT('Ctrl Pts',(89.4335148801687,-3.47221557776334,1.34722161762241));
#20537=CARTESIAN_POINT('Ctrl Pts',(89.4394684813942,-3.50940062625379,1.24216537021022));
#20538=CARTESIAN_POINT('Ctrl Pts',(89.445425610418,-3.54660770869388,1.13704687186226));
#20539=CARTESIAN_POINT('Ctrl Pts',(89.4513827394418,-3.57905530506113,1.03034686604588));
#20540=CARTESIAN_POINT('Ctrl Pts',(89.4573398684656,-3.60663242416782,0.922534616933895));
#20541=CARTESIAN_POINT('Ctrl Pts',(89.463305882831,-3.63425067586094,0.814561560718077));
#20542=CARTESIAN_POINT('Ctrl Pts',(89.4692718971964,-3.65698385982863,0.705473356159652));
#20543=CARTESIAN_POINT('Ctrl Pts',(89.4752379115619,-3.67477232943987,0.59574817606357));
#20544=CARTESIAN_POINT('Ctrl Pts',(89.4781531178931,-3.6834644069403,0.542132559319297));
#20545=CARTESIAN_POINT('Ctrl Pts',(89.4810683242243,-3.69097665121069,0.48836491923504));
#20546=CARTESIAN_POINT('Ctrl Pts',(89.4839835305554,-3.69730662674047,0.434501174176788));
#20547=CARTESIAN_POINT('Ctrl Pts',(89.4917410030471,-3.71415092709746,0.291167744869728));
#20548=CARTESIAN_POINT('Ctrl Pts',(89.4994984755388,-3.72266211806776,0.146836753085815));
#20549=CARTESIAN_POINT('Ctrl Pts',(89.5072559480305,-3.72274932293622,0.00224523449340528));
#20550=CARTESIAN_POINT('',(90.4429954109251,0.0296350623540759,3.72263204273257));
#20551=CARTESIAN_POINT('Ctrl Pts',(89.5072559480779,-3.72274932293675,0.00224523361020212));
#20552=CARTESIAN_POINT('Ctrl Pts',(89.5131410009605,-3.72281547915724,-0.107446258588759));
#20553=CARTESIAN_POINT('Ctrl Pts',(89.5190260538432,-3.71802930879369,-0.217318185000411));
#20554=CARTESIAN_POINT('Ctrl Pts',(89.5249111067258,-3.7083694126923,-0.326900384686496));
#20555=CARTESIAN_POINT('Ctrl Pts',(89.5307896394189,-3.69872021901865,-0.436361175657531));
#20556=CARTESIAN_POINT('Ctrl Pts',(89.5366681721121,-3.68420807032288,-0.545532453701019));
#20557=CARTESIAN_POINT('Ctrl Pts',(89.5425467048052,-3.66486360378298,-0.653943673542932));
#20558=CARTESIAN_POINT('Ctrl Pts',(89.5484203959138,-3.64553506942815,-0.762265605442191));
#20559=CARTESIAN_POINT('Ctrl Pts',(89.5542940870223,-3.62138220595615,-0.869828303288613));
#20560=CARTESIAN_POINT('Ctrl Pts',(89.5601677781308,-3.59248741612288,-0.976166854333197));
#20561=CARTESIAN_POINT('Ctrl Pts',(89.5660389041895,-3.56360524468848,-1.08245896717004));
#20562=CARTESIAN_POINT('Ctrl Pts',(89.5719100302482,-3.52998537330877,-1.18752758208424));
#20563=CARTESIAN_POINT('Ctrl Pts',(89.5777811563069,-3.49176103452334,-1.29091922298975));
#20564=CARTESIAN_POINT('Ctrl Pts',(89.5836512556447,-3.45354338026902,-1.3942927831472));
#20565=CARTESIAN_POINT('Ctrl Pts',(89.5895213549825,-3.41072300784237,-1.49598955000986));
#20566=CARTESIAN_POINT('Ctrl Pts',(89.5953914543204,-3.36348232776787,-1.59557331178897));
#20567=CARTESIAN_POINT('Ctrl Pts',(89.6012620640808,-3.31623753997572,-1.6951657326724));
#20568=CARTESIAN_POINT('Ctrl Pts',(89.6071326738412,-3.26457186568472,-1.7926443963283));
#20569=CARTESIAN_POINT('Ctrl Pts',(89.6130032836017,-3.20871455758169,-1.8875959447041));
#20570=CARTESIAN_POINT('Ctrl Pts',(89.618879452578,-3.15280435500192,-1.98263740812659));
#20571=CARTESIAN_POINT('Ctrl Pts',(89.6247556215542,-3.09269481009817,-2.07514660714444));
#20572=CARTESIAN_POINT('Ctrl Pts',(89.6306317905305,-3.02865953453122,-2.16473762530085));
#20573=CARTESIAN_POINT('Ctrl Pts',(89.6365108408342,-2.9645928598335,-2.25437257362028));
#20574=CARTESIAN_POINT('Ctrl Pts',(89.6423898911379,-2.89659688667175,-2.3410861548138));
#20575=CARTESIAN_POINT('Ctrl Pts',(89.6482689414417,-2.82498546918569,-2.4245256569873));
#20576=CARTESIAN_POINT('Ctrl Pts',(89.6541571245999,-2.75326280640904,-2.50809477887778));
#20577=CARTESIAN_POINT('Ctrl Pts',(89.6600453077582,-2.67791377583524,-2.58837935118275));
#20578=CARTESIAN_POINT('Ctrl Pts',(89.6659334909165,-2.59928914039452,-2.66506351277547));
#20579=CARTESIAN_POINT('Ctrl Pts',(89.6704777911736,-2.53860931073468,-2.72424575046689));
#20580=CARTESIAN_POINT('Ctrl Pts',(89.6750220914307,-2.47597921985387,-2.78128424885584));
#20581=CARTESIAN_POINT('Ctrl Pts',(89.6795663916879,-2.41157259940264,-2.8360509798504));
#20582=CARTESIAN_POINT('Ctrl Pts',(89.6855255449048,-2.32711318921056,-2.90786915266465));
#20583=CARTESIAN_POINT('Ctrl Pts',(89.6914846981217,-2.23930494820216,-2.97602838174629));
#20584=CARTESIAN_POINT('Ctrl Pts',(89.6974438513386,-2.14849817249947,-3.0402011718415));
#20585=CARTESIAN_POINT('Ctrl Pts',(89.7033954330532,-2.05780677287308,-3.10429242611883));
#20586=CARTESIAN_POINT('Ctrl Pts',(89.7093470147677,-1.96412475304399,-3.16440707422553));
#20587=CARTESIAN_POINT('Ctrl Pts',(89.7152985964823,-1.86783655449855,-3.22025684816894));
#20588=CARTESIAN_POINT('Ctrl Pts',(89.7212442421847,-1.77164439225896,-3.27605091844304));
#20589=CARTESIAN_POINT('Ctrl Pts',(89.727189887887,-1.67285158099827,-3.32758836649288));
#20590=CARTESIAN_POINT('Ctrl Pts',(89.7331355335894,-1.57187209771999,-3.37462378212881));
#20591=CARTESIAN_POINT('Ctrl Pts',(89.7390770554423,-1.47096265295516,-3.42162657439924));
#20592=CARTESIAN_POINT('Ctrl Pts',(89.7450185772952,-1.36786993061414,-3.4641333692047));
#20593=CARTESIAN_POINT('Ctrl Pts',(89.7509600991481,-1.26303248756112,-3.50194467372989));
#20594=CARTESIAN_POINT('Ctrl Pts',(89.7568994468785,-1.15823340663876,-3.53974214233767));
#20595=CARTESIAN_POINT('Ctrl Pts',(89.762838794609,-1.05169126684827,-3.57284739456322));
#20596=CARTESIAN_POINT('Ctrl Pts',(89.7687781423395,-0.943863968004348,
-3.60110932525008));
#20597=CARTESIAN_POINT('Ctrl Pts',(89.7747167859086,-0.836049453025415,
-3.62936790523902));
#20598=CARTESIAN_POINT('Ctrl Pts',(89.7806554294777,-0.726950486274686,
-3.65278419961963));
#20599=CARTESIAN_POINT('Ctrl Pts',(89.7865940730467,-0.617038715247114,
-3.6712573849277));
#20600=CARTESIAN_POINT('Ctrl Pts',(89.7925334815143,-0.507112787561259,
-3.68973294958577));
#20601=CARTESIAN_POINT('Ctrl Pts',(89.7984728899819,-0.396374259757346,
-3.70326407049529));
#20602=CARTESIAN_POINT('Ctrl Pts',(89.8044122984495,-0.285302749002038,
-3.71180143648766));
#20603=CARTESIAN_POINT('Ctrl Pts',(89.8103577330006,-0.174118545845956,
-3.72034746443361));
#20604=CARTESIAN_POINT('Ctrl Pts',(89.8163031675517,-0.0626011024771197,
-3.72388958443186));
#20605=CARTESIAN_POINT('Ctrl Pts',(89.8222486021027,0.0487669533004773,
-3.72243056977102));
#20606=CARTESIAN_POINT('Ctrl Pts',(89.828197013161,0.160190764097268,-3.7209708246728));
#20607=CARTESIAN_POINT('Ctrl Pts',(89.8341454242193,0.271464620812649,-3.71450498062451));
#20608=CARTESIAN_POINT('Ctrl Pts',(89.8400938352775,0.382109900634831,-3.70308784480423));
#20609=CARTESIAN_POINT('Ctrl Pts',(89.8460520730076,0.492937964538579,-3.69165184807376));
#20610=CARTESIAN_POINT('Ctrl Pts',(89.8520103107377,0.603134962393357,-3.67524827598416));
#20611=CARTESIAN_POINT('Ctrl Pts',(89.8579685484677,0.712230864897388,-3.65398340959391));
#20612=CARTESIAN_POINT('Ctrl Pts',(89.8636954499186,0.817090978010045,-3.63354417912029));
#20613=CARTESIAN_POINT('Ctrl Pts',(89.8694223513694,0.920933598171998,-3.60861424150156));
#20614=CARTESIAN_POINT('Ctrl Pts',(89.8751492528202,1.02335606424254,-3.57933093304852));
#20615=CARTESIAN_POINT('Ctrl Pts',(89.8811214150547,1.13016488382587,-3.54879353505999));
#20616=CARTESIAN_POINT('Ctrl Pts',(89.8870935772892,1.2357768263794,-3.5134222186467));
#20617=CARTESIAN_POINT('Ctrl Pts',(89.8930657395237,1.33972368461136,-3.47332808864803));
#20618=CARTESIAN_POINT('Ctrl Pts',(89.8990302904206,1.44353806576116,-3.43328505738812));
#20619=CARTESIAN_POINT('Ctrl Pts',(89.9049948413175,1.5456911979247,-3.38853133134063));
#20620=CARTESIAN_POINT('Ctrl Pts',(89.9109593922145,1.64572867738106,-3.33922815676701));
#20621=CARTESIAN_POINT('Ctrl Pts',(89.9169179513963,1.74566566375918,-3.28997450990847));
#20622=CARTESIAN_POINT('Ctrl Pts',(89.9228765105781,1.84349085378072,-3.23618068824731));
#20623=CARTESIAN_POINT('Ctrl Pts',(89.9288350697599,1.9387691973511,-3.17805625530804));
#20624=CARTESIAN_POINT('Ctrl Pts',(89.9347893692583,2.03397942788164,-3.11997337464254));
#20625=CARTESIAN_POINT('Ctrl Pts',(89.9407436687567,2.12664607998298,-3.05756625762786));
#20626=CARTESIAN_POINT('Ctrl Pts',(89.9466979682551,2.21635873816701,-2.99109035407671));
#20627=CARTESIAN_POINT('Ctrl Pts',(89.9526500068231,2.30603733120718,-2.92463969235056));
#20628=CARTESIAN_POINT('Ctrl Pts',(89.9586020453912,2.39276382656832,-2.85412356309229));
#20629=CARTESIAN_POINT('Ctrl Pts',(89.9645540839593,2.47615736440155,-2.77984033160539));
#20630=CARTESIAN_POINT('Ctrl Pts',(89.9705053172727,2.55953961987637,-2.70556714993846));
#20631=CARTESIAN_POINT('Ctrl Pts',(89.9764565505861,2.63958950407324,-2.62752815635622));
#20632=CARTESIAN_POINT('Ctrl Pts',(89.9824077838996,2.71596037037465,-2.54606104189479));
#20633=CARTESIAN_POINT('Ctrl Pts',(89.9883596666548,2.79233957081956,-2.46458503715026));
#20634=CARTESIAN_POINT('Ctrl Pts',(89.9943115494101,2.86503867095313,-2.37968047156783));
#20635=CARTESIAN_POINT('Ctrl Pts',(90.0002634321653,2.93374944851159,-2.29172025689392));
#20636=CARTESIAN_POINT('Ctrl Pts',(90.0062210830347,3.00252681535395,-2.20367479783893));
#20637=CARTESIAN_POINT('Ctrl Pts',(90.0121787339041,3.0673078817417,-2.11256810252635));
#20638=CARTESIAN_POINT('Ctrl Pts',(90.0181363847736,3.1278260792076,-2.01880449294348));
#20639=CARTESIAN_POINT('Ctrl Pts',(90.0240968896036,3.18837326738795,-1.92499596672158));
#20640=CARTESIAN_POINT('Ctrl Pts',(90.0300573944337,3.24465330725029,-1.82852834930477));
#20641=CARTESIAN_POINT('Ctrl Pts',(90.0360178992638,3.29644510455139,-1.72983156266128));
#20642=CARTESIAN_POINT('Ctrl Pts',(90.0419878953307,3.34831937275502,-1.6309776157435));
#20643=CARTESIAN_POINT('Ctrl Pts',(90.0479578913976,3.39569093916524,-1.5298877833216));
#20644=CARTESIAN_POINT('Ctrl Pts',(90.0539278874645,3.43838627710061,-1.42701344490732));
#20645=CARTESIAN_POINT('Ctrl Pts',(90.0595292962938,3.47844560715767,-1.33049056263903));
#20646=CARTESIAN_POINT('Ctrl Pts',(90.0651307051232,3.51438867417209,-1.23239716786626));
#20647=CARTESIAN_POINT('Ctrl Pts',(90.0707321139525,3.54611246929201,-1.13311690377988));
#20648=CARTESIAN_POINT('Ctrl Pts',(90.0767130680232,3.57998583353691,-1.02710951925937));
#20649=CARTESIAN_POINT('Ctrl Pts',(90.082694022094,3.6091539858786,-0.919418023660391));
#20650=CARTESIAN_POINT('Ctrl Pts',(90.0886749761647,3.63345076832199,-0.810495574744447));
#20651=CARTESIAN_POINT('Ctrl Pts',(90.0946484815713,3.65771729161799,-0.701708777552929));
#20652=CARTESIAN_POINT('Ctrl Pts',(90.1006219869779,3.6771244218003,-0.591694477428052));
#20653=CARTESIAN_POINT('Ctrl Pts',(90.1065954923845,3.69155544891906,-0.480921958384125));
#20654=CARTESIAN_POINT('Ctrl Pts',(90.1125631543477,3.70597235921939,-0.370257799994276));
#20655=CARTESIAN_POINT('Ctrl Pts',(90.1185308163109,3.71542279680153,-0.258837307097464));
#20656=CARTESIAN_POINT('Ctrl Pts',(90.124498478274,3.7198410318604,-0.147140273846959));
#20657=CARTESIAN_POINT('Ctrl Pts',(90.130462064005,3.7242562490285,-0.0355195356421509));
#20658=CARTESIAN_POINT('Ctrl Pts',(90.136425649736,3.72364608555073,0.076376954208075));
#20659=CARTESIAN_POINT('Ctrl Pts',(90.1423892354669,3.71799667388885,0.188064604462056));
#20660=CARTESIAN_POINT('Ctrl Pts',(90.1483506677351,3.71234930224091,0.299711924080306));
#20661=CARTESIAN_POINT('Ctrl Pts',(90.1543121000032,3.70166632145048,0.411150140640219));
#20662=CARTESIAN_POINT('Ctrl Pts',(90.1602735322713,3.6859859660511,0.521895603137585));
#20663=CARTESIAN_POINT('Ctrl Pts',(90.1662342543009,3.67030747879221,0.632627871540938));
#20664=CARTESIAN_POINT('Ctrl Pts',(90.1721949763305,3.64963285929706,0.742667139782877));
#20665=CARTESIAN_POINT('Ctrl Pts',(90.1781556983601,3.62405202518205,0.851536541361508));
#20666=CARTESIAN_POINT('Ctrl Pts',(90.1841171524673,3.59846804930732,0.960419313946667));
#20667=CARTESIAN_POINT('Ctrl Pts',(90.1900786065745,3.56797675585565,1.06813153082633));
#20668=CARTESIAN_POINT('Ctrl Pts',(90.1960400606817,3.53271865541614,1.17420886735485));
#20669=CARTESIAN_POINT('Ctrl Pts',(90.2020073510064,3.49742603756896,1.28039005277553));
#20670=CARTESIAN_POINT('Ctrl Pts',(90.2079746413311,3.45735742142443,1.3849327665398));
#20671=CARTESIAN_POINT('Ctrl Pts',(90.2139419316557,3.41270252760531,1.4873900028494));
#20672=CARTESIAN_POINT('Ctrl Pts',(90.2199121266179,3.36802589757602,1.58989711122969));
#20673=CARTESIAN_POINT('Ctrl Pts',(90.22588232158,3.31875872333222,1.69031634674488));
#20674=CARTESIAN_POINT('Ctrl Pts',(90.2318525165421,3.26513721747072,1.78822440246955));
#20675=CARTESIAN_POINT('Ctrl Pts',(90.2378321847936,3.21143062694341,1.88628781515534));
#20676=CARTESIAN_POINT('Ctrl Pts',(90.2438118530451,3.15335611271743,1.98183173031227));
#20677=CARTESIAN_POINT('Ctrl Pts',(90.2497915212967,3.09119409200401,2.0744605679693));
#20678=CARTESIAN_POINT('Ctrl Pts',(90.2552993392261,3.03393722125247,2.15978014614141));
#20679=CARTESIAN_POINT('Ctrl Pts',(90.2608071571555,2.97321311211844,2.24262669166008));
#20680=CARTESIAN_POINT('Ctrl Pts',(90.2663149750849,2.90927030595616,2.32271691115852));
#20681=CARTESIAN_POINT('Ctrl Pts',(90.2721536793902,2.8414860867939,2.40761861186677));
#20682=CARTESIAN_POINT('Ctrl Pts',(90.2779923836955,2.76984747689865,2.48971884002926));
#20683=CARTESIAN_POINT('Ctrl Pts',(90.2838310880009,2.69461904302155,2.56863694894503));
#20684=CARTESIAN_POINT('Ctrl Pts',(90.2896622591304,2.61948766989435,2.64745323664192));
#20685=CARTESIAN_POINT('Ctrl Pts',(90.2954934302599,2.54077597214089,2.72309524927075));
#20686=CARTESIAN_POINT('Ctrl Pts',(90.3013246013894,2.45879016274089,2.79521349776875));
#20687=CARTESIAN_POINT('Ctrl Pts',(90.3072275517867,2.37579514245696,2.86821949161985));
#20688=CARTESIAN_POINT('Ctrl Pts',(90.313130502184,2.2894451207709,2.93761401254684));
#20689=CARTESIAN_POINT('Ctrl Pts',(90.3190334525814,2.20009821870295,3.00307099326009));
#20690=CARTESIAN_POINT('Ctrl Pts',(90.3248549934603,2.11198352896493,3.06762523535735));
#20691=CARTESIAN_POINT('Ctrl Pts',(90.3306765343393,2.02095446068037,3.12834959116476));
#20692=CARTESIAN_POINT('Ctrl Pts',(90.3364980752183,1.92738871149693,3.18497100729257));
#20693=CARTESIAN_POINT('Ctrl Pts',(90.3423177972162,1.83385219597801,3.2415747326361));
#20694=CARTESIAN_POINT('Ctrl Pts',(90.348137519214,1.73778094652395,3.29407783912181));
#20695=CARTESIAN_POINT('Ctrl Pts',(90.3539572412119,1.63958106793698,3.34225096067944));
#20696=CARTESIAN_POINT('Ctrl Pts',(90.3597767137142,1.54138539924807,3.39042201702136));
#20697=CARTESIAN_POINT('Ctrl Pts',(90.3655961862165,1.4410616746966,3.434263266282));
#20698=CARTESIAN_POINT('Ctrl Pts',(90.3714156587188,1.33903905919695,3.47359208319643));
#20699=CARTESIAN_POINT('Ctrl Pts',(90.3773806380693,1.23446552705938,3.51390425593767));
#20700=CARTESIAN_POINT('Ctrl Pts',(90.3833456174198,1.12810746066854,3.54947515349255));
#20701=CARTESIAN_POINT('Ctrl Pts',(90.3893105967704,1.02044559762071,3.58016177634426));
#20702=CARTESIAN_POINT('Ctrl Pts',(90.3951373490544,0.915278593754489,3.61013729499801));
#20703=CARTESIAN_POINT('Ctrl Pts',(90.4009641013384,0.80886800737136,3.63545240450293));
#20704=CARTESIAN_POINT('Ctrl Pts',(90.4067908536225,0.701672758016952,3.65602556106449));
#20705=CARTESIAN_POINT('Ctrl Pts',(90.4128249465063,0.590663046299211,3.67733079793624));
#20706=CARTESIAN_POINT('Ctrl Pts',(90.41885903939,0.47881230049198,3.69355024052747));
#20707=CARTESIAN_POINT('Ctrl Pts',(90.4248931322738,0.36663482167895,3.70465200390434));
#20708=CARTESIAN_POINT('Ctrl Pts',(90.4309272251575,0.254457342865911,3.71575376728122));
#20709=CARTESIAN_POINT('Ctrl Pts',(90.4369613180413,0.141953645119487,3.72173789897472));
#20710=CARTESIAN_POINT('Ctrl Pts',(90.4429954109251,0.029635062354076,3.72263204273257));
#20711=CARTESIAN_POINT('',(90.4430005297901,3.5302572329849,1.18158852036477));
#20712=CARTESIAN_POINT('Origin',(90.4430005297901,0.,0.));
#20713=CARTESIAN_POINT('',(89.7537451115497,-3.72274996600548,0.000503096633030775));
#20714=CARTESIAN_POINT('Ctrl Pts',(89.7537451115497,-3.72274996600548,0.000503096633030831));
#20715=CARTESIAN_POINT('Ctrl Pts',(89.7599512036108,-3.7227657376518,-0.11620190985295));
#20716=CARTESIAN_POINT('Ctrl Pts',(89.7661572956718,-3.71728927921443,-0.232822253785277));
#20717=CARTESIAN_POINT('Ctrl Pts',(89.7723633877328,-3.70637040353398,-0.348835196485874));
#20718=CARTESIAN_POINT('Ctrl Pts',(89.7785765674432,-3.6954390579834,-0.464980631429494));
#20719=CARTESIAN_POINT('Ctrl Pts',(89.7847897471536,-3.67905293405017,-0.580516922988185));
#20720=CARTESIAN_POINT('Ctrl Pts',(89.791002926864,-3.65731331519107,-0.694929404347014));
#20721=CARTESIAN_POINT('Ctrl Pts',(89.7972291983796,-3.63552788873094,-0.809582964509177));
#20722=CARTESIAN_POINT('Ctrl Pts',(89.8034554698953,-3.60836649028465,-0.923107626647784));
#20723=CARTESIAN_POINT('Ctrl Pts',(89.809681741411,-3.57598115751633,-1.03500063941437));
#20724=CARTESIAN_POINT('Ctrl Pts',(89.8159150699073,-3.543559118564,-1.14702047395997));
#20725=CARTESIAN_POINT('Ctrl Pts',(89.8221483984037,-3.50590144927669,-1.25740462855842));
#20726=CARTESIAN_POINT('Ctrl Pts',(89.8283817269001,-3.46320891153749,-1.36566891944839));
#20727=CARTESIAN_POINT('Ctrl Pts',(89.8346278435039,-3.42042878708434,-1.4741553220698));
#20728=CARTESIAN_POINT('Ctrl Pts',(89.8408739601077,-3.37259329515473,-1.58051283856969));
#20729=CARTESIAN_POINT('Ctrl Pts',(89.8471200767115,-3.31995031615005,-1.6842795079188));
#20730=CARTESIAN_POINT('Ctrl Pts',(89.850164033272,-3.29429550509387,-1.73484872619658));
#20731=CARTESIAN_POINT('Ctrl Pts',(89.8532079898325,-3.26749960874441,-1.78480303788735));
#20732=CARTESIAN_POINT('Ctrl Pts',(89.856251946393,-3.23959504134923,-1.83409147279122));
#20733=CARTESIAN_POINT('Ctrl Pts',(89.8621583025938,-3.18545027568409,-1.92972853177436));
#20734=CARTESIAN_POINT('Ctrl Pts',(89.8680646587945,-3.12696964229294,-2.02313739625222));
#20735=CARTESIAN_POINT('Ctrl Pts',(89.8739710149952,-3.06436251000767,-2.11389450298719));
#20736=CARTESIAN_POINT('Ctrl Pts',(89.8798697866757,-3.001835773325,-2.20453506593522));
#20737=CARTESIAN_POINT('Ctrl Pts',(89.8857685583561,-2.93519330999383,-2.29253029220606));
#20738=CARTESIAN_POINT('Ctrl Pts',(89.8916673300365,-2.86469027909109,-2.37748126541115));
#20739=CARTESIAN_POINT('Ctrl Pts',(89.8975602106855,-2.79425765870664,-2.46234739911394));
#20740=CARTESIAN_POINT('Ctrl Pts',(89.9034530913345,-2.7199724064974,-2.54417499829643));
#20741=CARTESIAN_POINT('Ctrl Pts',(89.9093459719835,-2.64213238104237,-2.62259490649001));
#20742=CARTESIAN_POINT('Ctrl Pts',(89.9152830067977,-2.56370911598825,-2.701602399227));
#20743=CARTESIAN_POINT('Ctrl Pts',(89.921220041612,-2.48167783266002,-2.77715055978529));
#20744=CARTESIAN_POINT('Ctrl Pts',(89.9271570764262,-2.39638394500998,-2.84889654964837));
#20745=CARTESIAN_POINT('Ctrl Pts',(89.9330440800188,-2.31180882649886,-2.92003793811767));
#20746=CARTESIAN_POINT('Ctrl Pts',(89.9389310836114,-2.22402622323072,-2.98744072580214));
#20747=CARTESIAN_POINT('Ctrl Pts',(89.9448180872039,-2.13340829389835,-3.05080917364979));
#20748=CARTESIAN_POINT('Ctrl Pts',(89.9507046169406,-2.04279765857208,-3.11417252085292));
#20749=CARTESIAN_POINT('Ctrl Pts',(89.9565911466773,-1.94935249985621,-3.1735019293205));
#20750=CARTESIAN_POINT('Ctrl Pts',(89.9624776764139,-1.85347519871799,-3.22854413787969));
#20751=CARTESIAN_POINT('Ctrl Pts',(89.9683652527117,-1.7575808516366,-3.28359613234594));
#20752=CARTESIAN_POINT('Ctrl Pts',(89.9742528290094,-1.65925387239635,-3.33435920010058));
#20753=CARTESIAN_POINT('Ctrl Pts',(89.9801404053071,-1.55892176495189,-3.38062575468792));
#20754=CARTESIAN_POINT('Ctrl Pts',(89.9861149388253,-1.45710779115981,-3.42757564835794));
#20755=CARTESIAN_POINT('Ctrl Pts',(89.9920894723435,-1.35322939292269,-3.46989494412881));
#20756=CARTESIAN_POINT('Ctrl Pts',(89.9980640058617,-1.24775336896973,-3.5074177242987));
#20757=CARTESIAN_POINT('Ctrl Pts',(90.0039617045284,-1.14363380817999,-3.54445794675382));
#20758=CARTESIAN_POINT('Ctrl Pts',(90.0098594031951,-1.03795790361118,-3.57682424444751));
#20759=CARTESIAN_POINT('Ctrl Pts',(90.0157571018618,-0.931187775105836,
-3.60440798051406));
#20760=CARTESIAN_POINT('Ctrl Pts',(90.0217700528058,-0.822331154708589,
-3.63253075537785));
#20761=CARTESIAN_POINT('Ctrl Pts',(90.0277830037497,-0.712337557539733,
-3.65568200449768));
#20762=CARTESIAN_POINT('Ctrl Pts',(90.0337959546936,-0.601703826612937,
-3.67380185469213));
#20763=CARTESIAN_POINT('Ctrl Pts',(90.0398089056375,-0.491070095686133,
-3.69192170488658));
#20764=CARTESIAN_POINT('Ctrl Pts',(90.0458218565815,-0.379796697029761,
-3.70501017755296));
#20765=CARTESIAN_POINT('Ctrl Pts',(90.0518348075254,-0.268380670821446,
-3.71306334150516));
#20766=CARTESIAN_POINT('Ctrl Pts',(90.0578840925175,-0.156291398598147,
-3.72116516776137));
#20767=CARTESIAN_POINT('Ctrl Pts',(90.0639333775095,-0.043666389847885,
-3.7241992834387));
#20768=CARTESIAN_POINT('Ctrl Pts',(90.0699826625016,0.0690062792362871,
-3.72211038201797));
#20769=CARTESIAN_POINT('Ctrl Pts',(90.0760236191776,0.181523826912398,-3.72002435647949));
#20770=CARTESIAN_POINT('Ctrl Pts',(90.0820645758535,0.29408850410863,-3.71282935507544));
#20771=CARTESIAN_POINT('Ctrl Pts',(90.0881055325295,0.406208228326725,-3.70052191423584));
#20772=CARTESIAN_POINT('Ctrl Pts',(90.0941396621041,0.518201242032032,-3.68822838247558));
#20773=CARTESIAN_POINT('Ctrl Pts',(90.1001737916788,0.629749904560712,-3.67083395347465));
#20774=CARTESIAN_POINT('Ctrl Pts',(90.1062079212534,0.740363809626243,-3.64838717680782));
#20775=CARTESIAN_POINT('Ctrl Pts',(90.1122361716886,0.850869941968559,-3.62596227035926));
#20776=CARTESIAN_POINT('Ctrl Pts',(90.1182644221237,0.960442736497499,-3.59849489909187));
#20777=CARTESIAN_POINT('Ctrl Pts',(90.1242926725589,1.06859925975183,-3.56608513422743));
#20778=CARTESIAN_POINT('Ctrl Pts',(90.1303176185233,1.17669649547857,-3.53369313523388));
#20779=CARTESIAN_POINT('Ctrl Pts',(90.1363425644877,1.28337861886902,-3.49636424846651));
#20780=CARTESIAN_POINT('Ctrl Pts',(90.1423675104521,1.38817548640195,-3.45424903292347));
#20781=CARTESIAN_POINT('Ctrl Pts',(90.1483904990954,1.49293830862879,-3.41214749932949));
#20782=CARTESIAN_POINT('Ctrl Pts',(90.1544134877387,1.59581671987081,-3.36526288194251));
#20783=CARTESIAN_POINT('Ctrl Pts',(90.1604364763819,1.69635882928629,-3.31379454474813));
#20784=CARTESIAN_POINT('Ctrl Pts',(90.166458852972,1.7968907216628,-3.26233143774048));
#20785=CARTESIAN_POINT('Ctrl Pts',(90.1724812295622,1.89508642622163,-3.20628572291655));
#20786=CARTESIAN_POINT('Ctrl Pts',(90.1785036061523,1.9905175443936,-3.14590328331328));
#20787=CARTESIAN_POINT('Ctrl Pts',(90.1845293098987,2.08600138498086,-3.08548748448591));
#20788=CARTESIAN_POINT('Ctrl Pts',(90.1905550136451,2.17871724465894,-3.02073038761758));
#20789=CARTESIAN_POINT('Ctrl Pts',(90.1965807173915,2.26826465617017,-2.95192191835577));
#20790=CARTESIAN_POINT('Ctrl Pts',(90.2026080049839,2.35783560506721,-2.88309536290408));
#20791=CARTESIAN_POINT('Ctrl Pts',(90.2086352925763,2.44423613268206,-2.81021556759798));
#20792=CARTESIAN_POINT('Ctrl Pts',(90.2146625801687,2.52709895717264,-2.73361270540597));
#20793=CARTESIAN_POINT('Ctrl Pts',(90.2206965450462,2.61005358061807,-2.65692497931112));
#20794=CARTESIAN_POINT('Ctrl Pts',(90.2267305099237,2.6894623804383,-2.57650622715388));
#20795=CARTESIAN_POINT('Ctrl Pts',(90.2327644748012,2.76499482777154,-2.49272364390773));
#20796=CARTESIAN_POINT('Ctrl Pts',(90.2376488727534,2.82613713445795,-2.42490298430147));
#20797=CARTESIAN_POINT('Ctrl Pts',(90.2425332707056,2.88474007503412,-2.35487887900625));
#20798=CARTESIAN_POINT('Ctrl Pts',(90.2474176686577,2.94064827745286,-2.28286120270452));
#20799=CARTESIAN_POINT('Ctrl Pts',(90.2534516475349,3.00971490874737,-2.1938936079576));
#20800=CARTESIAN_POINT('Ctrl Pts',(90.2594856264121,3.07480863629318,-2.10170138960284));
#20801=CARTESIAN_POINT('Ctrl Pts',(90.2655196052893,3.13562421825931,-2.00667095567901));
#20802=CARTESIAN_POINT('Ctrl Pts',(90.2715487836387,3.19639141641505,-1.91171612630169));
#20803=CARTESIAN_POINT('Ctrl Pts',(90.2775779619882,3.25288702530268,-1.81392791401824));
#20804=CARTESIAN_POINT('Ctrl Pts',(90.2836071403376,3.30484797888165,-1.71372325624118));
#20805=CARTESIAN_POINT('Ctrl Pts',(90.289632992101,3.35678026311715,-1.61357388616678));
#20806=CARTESIAN_POINT('Ctrl Pts',(90.2956588438643,3.40418268650556,-1.51101108237129));
#20807=CARTESIAN_POINT('Ctrl Pts',(90.3016846956277,3.44683746281631,-1.40647753889851));
#20808=CARTESIAN_POINT('Ctrl Pts',(90.3077085814766,3.48947832314596,-1.30197809915199));
#20809=CARTESIAN_POINT('Ctrl Pts',(90.3137324673256,3.5273744688306,-1.19550957398247));
#20810=CARTESIAN_POINT('Ctrl Pts',(90.3197563531745,3.56035595604716,-1.08753529999698));
#20811=CARTESIAN_POINT('Ctrl Pts',(90.3257805290223,3.5933390310418,-0.97955582796857));
#20812=CARTESIAN_POINT('Ctrl Pts',(90.3318047048702,3.62140685386691,-0.870070847711997));
#20813=CARTESIAN_POINT('Ctrl Pts',(90.337828880718,3.6444392446607,-0.75955918431481));
#20814=CARTESIAN_POINT('Ctrl Pts',(90.3402889535533,3.65384490617449,-0.714429900579265));
#20815=CARTESIAN_POINT('Ctrl Pts',(90.3427490263886,3.66241142849172,-0.669129549522075));
#20816=CARTESIAN_POINT('Ctrl Pts',(90.3452090992239,3.67013307523028,-0.623691247814765));
#20817=CARTESIAN_POINT('Ctrl Pts',(90.3519493338375,3.69128924177713,-0.499197041970545));
#20818=CARTESIAN_POINT('Ctrl Pts',(90.3586895684512,3.70608966530002,-0.37372607149069));
#20819=CARTESIAN_POINT('Ctrl Pts',(90.3654298030648,3.71448732777005,-0.247894038524024));
#20820=CARTESIAN_POINT('Ctrl Pts',(90.3721853209071,3.72290403162413,-0.121776686151497));
#20821=CARTESIAN_POINT('Ctrl Pts',(90.3789408387494,3.72488891581502,0.00470315930204165));
#20822=CARTESIAN_POINT('Ctrl Pts',(90.3856963565917,3.72044700092353,0.130926222809181));
#20823=CARTESIAN_POINT('Ctrl Pts',(90.3924547873692,3.7160031707073,0.25720371287845));
#20824=CARTESIAN_POINT('Ctrl Pts',(90.3992132181468,3.70512702164482,0.383223993907095));
#20825=CARTESIAN_POINT('Ctrl Pts',(90.4059716489243,3.68787564481499,0.508370721895352));
#20826=CARTESIAN_POINT('Ctrl Pts',(90.4127260755569,3.67063448885085,0.633443304619199));
#20827=CARTESIAN_POINT('Ctrl Pts',(90.4194805021895,3.64702568694021,0.757643165561556));
#20828=CARTESIAN_POINT('Ctrl Pts',(90.4262349288221,3.6171578044059,0.88036184635948));
#20829=CARTESIAN_POINT('Ctrl Pts',(90.4318234624781,3.59244546746669,0.981897848623131));
#20830=CARTESIAN_POINT('Ctrl Pts',(90.4374119961341,3.56344927633744,1.082419944246));
#20831=CARTESIAN_POINT('Ctrl Pts',(90.4430005297901,3.5302572329849,1.18158852036477));
#20832=CARTESIAN_POINT('Ctrl Pts',(89.7566589927103,-3.72274994160873,0.000659357419522499));
#20833=CARTESIAN_POINT('Ctrl Pts',(89.7548842680598,-3.72274408006351,0.0337538012808603));
#20834=CARTESIAN_POINT('Ctrl Pts',(89.7530965611029,-3.72229691578573,0.0668461131889498));
#20835=CARTESIAN_POINT('Ctrl Pts',(89.7488269168412,-3.72019059588082,0.145287725484996));
#20836=CARTESIAN_POINT('Ctrl Pts',(89.7463339333092,-3.7181433796351,0.190620476795769));
#20837=CARTESIAN_POINT('Ctrl Pts',(89.7266764545911,-3.69567992210142,0.54440014442492));
#20838=CARTESIAN_POINT('Ctrl Pts',(89.708392504169,-3.6377447484145,0.849223948899964));
#20839=CARTESIAN_POINT('Ctrl Pts',(89.6849660701368,-3.51479749359358,1.23020361268767));
#20840=CARTESIAN_POINT('Ctrl Pts',(89.679660158538,-3.48357147177563,1.31602944805247));
#20841=CARTESIAN_POINT('Ctrl Pts',(89.6709090180228,-3.42585376385813,1.45816693176171));
#20842=CARTESIAN_POINT('Ctrl Pts',(89.6674128539193,-3.40104952542244,1.51511970867108));
#20843=CARTESIAN_POINT('Ctrl Pts',(89.6623070451736,-3.36199869035049,1.59898607879666));
#20844=CARTESIAN_POINT('Ctrl Pts',(89.6606458111315,-3.34882924909552,1.62638693204885));
#20845=CARTESIAN_POINT('Ctrl Pts',(89.6576145772363,-3.32390150226231,1.67666567167764));
#20846=CARTESIAN_POINT('Ctrl Pts',(89.6562397927448,-3.31223993366645,1.69958690024722));
#20847=CARTESIAN_POINT('Ctrl Pts',(89.652861576564,-3.28270889279143,1.75617260522631));
#20848=CARTESIAN_POINT('Ctrl Pts',(89.6508741592126,-3.26455855763923,1.78968643437814));
#20849=CARTESIAN_POINT('Ctrl Pts',(89.642385997097,-3.1838545696962,1.93338841465287));
#20850=CARTESIAN_POINT('Ctrl Pts',(89.636136557727,-3.11620874804651,2.04062945968947));
#20851=CARTESIAN_POINT('Ctrl Pts',(89.6193872732306,-2.91743945728341,2.32273632390737));
#20852=CARTESIAN_POINT('Ctrl Pts',(89.6090943159204,-2.77619621897553,2.48983778588698));
#20853=CARTESIAN_POINT('Ctrl Pts',(89.5984125828405,-2.62112000708803,2.64359555736933));
#20854=CARTESIAN_POINT('Ctrl Pts',(90.1028989154209,-1.84736391785682,1.20202435615052));
#20855=CARTESIAN_POINT('Ctrl Pts',(90.140690073821,-2.22792678283258,0.617153363646938));
#20856=CARTESIAN_POINT('Ctrl Pts',(90.2162692554159,-2.38778162526882,-0.933200414266254));
#20857=CARTESIAN_POINT('Ctrl Pts',(90.3296364602056,-0.62872205324772,-2.48534112021196));
#20858=CARTESIAN_POINT('Ctrl Pts',(90.4052125065953,0.88959187531312,-2.13379067845246));
#20859=CARTESIAN_POINT('Ctrl Pts',(90.4430005297901,1.42252785196827,-1.68345790276281));
#20860=CARTESIAN_POINT('Ctrl Pts',(90.1853507684723,-1.72766177787012,1.12413775981909));
#20861=CARTESIAN_POINT('Ctrl Pts',(90.2231419268724,-2.08356561984736,0.577164178184089));
#20862=CARTESIAN_POINT('Ctrl Pts',(90.2987211084673,-2.23306247783782,-0.872732584650031));
#20863=CARTESIAN_POINT('Ctrl Pts',(90.4120883132569,-0.587983260796952,
-2.32430048939166));
#20864=CARTESIAN_POINT('Ctrl Pts',(90.4876643596466,0.831949712791466,-1.99552917619753));
#20865=CARTESIAN_POINT('Ctrl Pts',(90.5254523828415,1.33035346963605,-1.5743762477676));
#20866=CARTESIAN_POINT('Ctrl Pts',(90.2678026215237,-1.60795963788343,1.04625116348766));
#20867=CARTESIAN_POINT('Ctrl Pts',(90.3055937799238,-1.93920445686214,0.537174992721241));
#20868=CARTESIAN_POINT('Ctrl Pts',(90.3811729615186,-2.07834333040681,-0.812264755033806));
#20869=CARTESIAN_POINT('Ctrl Pts',(90.4945401663084,-0.547244468346182,
-2.16325985857137));
#20870=CARTESIAN_POINT('Ctrl Pts',(90.5701162126981,0.774307550269809,-1.85726767394259));
#20871=CARTESIAN_POINT('Ctrl Pts',(90.6079042358929,1.23817908730384,-1.4652945927724));
#20872=CARTESIAN_POINT('Ctrl Pts',(90.3502544745751,-1.48825749789673,0.968364567156219));
#20873=CARTESIAN_POINT('Ctrl Pts',(90.3880456329751,-1.79484329387692,0.497185807258393));
#20874=CARTESIAN_POINT('Ctrl Pts',(90.4636248145701,-1.92362418297579,-0.751796925417581));
#20875=CARTESIAN_POINT('Ctrl Pts',(90.5769920193598,-0.506505675895414,
-2.00221922775108));
#20876=CARTESIAN_POINT('Ctrl Pts',(90.6525680657495,0.716665387748153,-1.71900617168766));
#20877=CARTESIAN_POINT('Ctrl Pts',(90.6903560889443,1.14600470497162,-1.35621293777719));
#20878=CARTESIAN_POINT('',(90.4430005297901,1.42252785196811,-1.68345790276294));
#20879=CARTESIAN_POINT('',(90.4428667905869,-1.7396164773305,-0.358885182614483));
#20880=CARTESIAN_POINT('Ctrl Pts',(90.4430005297901,1.4225278519681,-1.68345790276293));
#20881=CARTESIAN_POINT('Ctrl Pts',(90.4430005297901,1.35849356753156,-1.72802743598208));
#20882=CARTESIAN_POINT('Ctrl Pts',(90.4430005297901,1.29211327677448,-1.7687933284719));
#20883=CARTESIAN_POINT('Ctrl Pts',(90.4430005297901,1.22375356660468,-1.80575874571043));
#20884=CARTESIAN_POINT('Ctrl Pts',(90.4430005297901,1.15444662535534,-1.84323637682451));
#20885=CARTESIAN_POINT('Ctrl Pts',(90.4430005297901,1.08310399461725,-1.87680762782933));
#20886=CARTESIAN_POINT('Ctrl Pts',(90.4430005297901,1.01008882142485,-1.90642508439205));
#20887=CARTESIAN_POINT('Ctrl Pts',(90.4430005297901,0.937375387734288,-1.93592014507186));
#20888=CARTESIAN_POINT('Ctrl Pts',(90.4430005297901,0.863002156171073,-1.96149402884632));
#20889=CARTESIAN_POINT('Ctrl Pts',(90.4430005297901,0.787324930426492,-1.98304902266566));
#20890=CARTESIAN_POINT('Ctrl Pts',(90.4430005297901,0.744830143821219,-1.99515272828672));
#20891=CARTESIAN_POINT('Ctrl Pts',(90.4430005297901,0.701924229083204,-2.0059883116318));
#20892=CARTESIAN_POINT('Ctrl Pts',(90.4430005297901,0.658671653783695,-2.0155313726465));
#20893=CARTESIAN_POINT('Ctrl Pts',(90.4430005297901,0.646172907588059,-2.01828904191188));
#20894=CARTESIAN_POINT('Ctrl Pts',(90.4430005297901,0.633654218360875,-2.02093674442495));
#20895=CARTESIAN_POINT('Ctrl Pts',(90.4430005297901,0.6211203149044,-2.02347372260163));
#20896=CARTESIAN_POINT('Ctrl Pts',(90.4430005297901,0.545600596598426,-2.0387596132195));
#20897=CARTESIAN_POINT('Ctrl Pts',(90.4430005297901,0.469491648685046,-2.0500382632572));
#20898=CARTESIAN_POINT('Ctrl Pts',(90.4430005297901,0.393135312093146,-2.05726598238603));
#20899=CARTESIAN_POINT('Ctrl Pts',(90.4430005297901,0.317994445849382,-2.06437864782478));
#20900=CARTESIAN_POINT('Ctrl Pts',(90.4430005297901,0.242613051514531,-2.06756819235912));
#20901=CARTESIAN_POINT('Ctrl Pts',(90.4430005297901,0.167322657723717,-2.06674371029438));
#20902=CARTESIAN_POINT('Ctrl Pts',(90.4430005297901,0.111038822526298,-2.06612736323709));
#20903=CARTESIAN_POINT('Ctrl Pts',(90.4430005297901,0.0548058830297967,
-2.0632668109814));
#20904=CARTESIAN_POINT('Ctrl Pts',(90.4430005297901,-0.00123083108011989,
-2.05810621712316));
#20905=CARTESIAN_POINT('Ctrl Pts',(90.4430005297901,-0.0254665698698807,
-2.05587427317829));
#20906=CARTESIAN_POINT('Ctrl Pts',(90.4430005297901,-0.0496655066289073,
-2.05321190325344));
#20907=CARTESIAN_POINT('Ctrl Pts',(90.4430005297901,-0.0738153724767186,
-2.05011370335277));
#20908=CARTESIAN_POINT('Ctrl Pts',(90.4430005297901,-0.0915898373131226,
-2.04783340724109));
#20909=CARTESIAN_POINT('Ctrl Pts',(90.4430005297901,-0.109337713577794,
-2.04531700834962));
#20910=CARTESIAN_POINT('Ctrl Pts',(90.4430005297901,-0.12705398082619,-2.04256216657337));
#20911=CARTESIAN_POINT('Ctrl Pts',(90.4430005297901,-0.141731501026051,
-2.04027984348287));
#20912=CARTESIAN_POINT('Ctrl Pts',(90.4430005297901,-0.156389839833323,
-2.03783328837979));
#20913=CARTESIAN_POINT('Ctrl Pts',(90.4430005297901,-0.171003090990929,
-2.03522554868848));
#20914=CARTESIAN_POINT('Ctrl Pts',(90.4430005297901,-0.242576842352592,
-2.02245318815975));
#20915=CARTESIAN_POINT('Ctrl Pts',(90.4430005297901,-0.313187615395148,
-2.00580133374315));
#20916=CARTESIAN_POINT('Ctrl Pts',(90.4430005297901,-0.382533842296707,
-1.98519475375429));
#20917=CARTESIAN_POINT('Ctrl Pts',(90.4430005297901,-0.42007629343071,-1.97403882564058));
#20918=CARTESIAN_POINT('Ctrl Pts',(90.4430005297901,-0.457247853160681,
-1.96172298204887));
#20919=CARTESIAN_POINT('Ctrl Pts',(90.4430005297901,-0.493997977180846,
-1.94822944989875));
#20920=CARTESIAN_POINT('Ctrl Pts',(90.4430005297901,-0.563441751304489,
-1.92273179992486));
#20921=CARTESIAN_POINT('Ctrl Pts',(90.4430005297901,-0.631383008777137,
-1.89303101435383));
#20922=CARTESIAN_POINT('Ctrl Pts',(90.4430005297901,-0.697549630821063,
-1.85938942477736));
#20923=CARTESIAN_POINT('Ctrl Pts',(90.4430005297901,-0.728482655886315,
-1.84366191592987));
#20924=CARTESIAN_POINT('Ctrl Pts',(90.4430005297901,-0.759027301881822,
-1.82707257188128));
#20925=CARTESIAN_POINT('Ctrl Pts',(90.4430005297901,-0.789152711196381,
-1.80964576389468));
#20926=CARTESIAN_POINT('Ctrl Pts',(90.4430005297901,-0.805665241648401,
-1.80009367135528));
#20927=CARTESIAN_POINT('Ctrl Pts',(90.4430005297901,-0.822051778690102,
-1.79028994553457));
#20928=CARTESIAN_POINT('Ctrl Pts',(90.4430005297901,-0.838306956091588,
-1.78023844910883));
#20929=CARTESIAN_POINT('Ctrl Pts',(90.4430005297901,-0.848486765356263,
-1.77394369674094));
#20930=CARTESIAN_POINT('Ctrl Pts',(90.4430005297901,-0.858617377556729,
-1.76755026518767));
#20931=CARTESIAN_POINT('Ctrl Pts',(90.4430005297901,-0.868689640147188,
-1.76106412386971));
#20932=CARTESIAN_POINT('Ctrl Pts',(90.4430005297901,-0.929470414251205,
-1.72192369373168));
#20933=CARTESIAN_POINT('Ctrl Pts',(90.4430005297901,-0.98799906476567,-1.67949685006462));
#20934=CARTESIAN_POINT('Ctrl Pts',(90.4430005297901,-1.04404927334162,-1.63406019156795));
#20935=CARTESIAN_POINT('Ctrl Pts',(90.4430005297901,-1.09986300683067,-1.5888152297311));
#20936=CARTESIAN_POINT('Ctrl Pts',(90.4430005297901,-1.15321978054266,-1.54058487743322));
#20937=CARTESIAN_POINT('Ctrl Pts',(90.4430005297901,-1.20385708288004,-1.48960963106486));
#20938=CARTESIAN_POINT('Ctrl Pts',(90.4430005297901,-1.25409004216062,-1.43904142626441));
#20939=CARTESIAN_POINT('Ctrl Pts',(90.4430005297901,-1.30164732632187,-1.38577112858578));
#20940=CARTESIAN_POINT('Ctrl Pts',(90.4430005297901,-1.34622563323271,-1.3300145930638));
#20941=CARTESIAN_POINT('Ctrl Pts',(90.4430005297901,-1.36342852935171,-1.30849798655699));
#20942=CARTESIAN_POINT('Ctrl Pts',(90.4430005297901,-1.38018725088433,-1.28661099372197));
#20943=CARTESIAN_POINT('Ctrl Pts',(90.4430005297901,-1.39648221326537,-1.26436566883623));
#20944=CARTESIAN_POINT('Ctrl Pts',(90.4430005297901,-1.40413618854342,-1.25391672377294));
#20945=CARTESIAN_POINT('Ctrl Pts',(90.4430005297901,-1.41168748957156,-1.24338902200558));
#20946=CARTESIAN_POINT('Ctrl Pts',(90.4430005297901,-1.41912637484512,-1.2327951746032));
#20947=CARTESIAN_POINT('Ctrl Pts',(90.4430005297901,-1.45875449510069,-1.17636007130584));
#20948=CARTESIAN_POINT('Ctrl Pts',(90.4430005297901,-1.49525634166901,-1.11796797580368));
#20949=CARTESIAN_POINT('Ctrl Pts',(90.4430005297901,-1.52837656473231,-1.05783238657754));
#20950=CARTESIAN_POINT('Ctrl Pts',(90.4430005297901,-1.5611740548108,-0.998282775838552));
#20951=CARTESIAN_POINT('Ctrl Pts',(90.4430005297902,-1.59065591048662,-0.937022733178433));
#20952=CARTESIAN_POINT('Ctrl Pts',(90.4430005297902,-1.616524485471,-0.874251203149238));
#20953=CARTESIAN_POINT('Ctrl Pts',(90.4430005297902,-1.62298306524415,-0.858579101596652));
#20954=CARTESIAN_POINT('Ctrl Pts',(90.4430005297902,-1.62921615191983,-0.842812771601484));
#20955=CARTESIAN_POINT('Ctrl Pts',(90.4430005297902,-1.63521857834345,-0.826955310014826));
#20956=CARTESIAN_POINT('Ctrl Pts',(90.4430005297902,-1.64047153672405,-0.813077824501807));
#20957=CARTESIAN_POINT('Ctrl Pts',(90.4430005297902,-1.64554478527699,-0.799138477894352));
#20958=CARTESIAN_POINT('Ctrl Pts',(90.4430005297902,-1.65043379611914,-0.785144399166619));
#20959=CARTESIAN_POINT('Ctrl Pts',(90.4430005297902,-1.66472446959871,-0.74423943572875));
#20960=CARTESIAN_POINT('Ctrl Pts',(90.4430005297902,-1.6774468220569,-0.702853420185196));
#20961=CARTESIAN_POINT('Ctrl Pts',(90.4430005297902,-1.6885285201336,-0.661040028896644));
#20962=CARTESIAN_POINT('Ctrl Pts',(90.4430005297902,-1.70605020045711,-0.594927338374926));
#20963=CARTESIAN_POINT('Ctrl Pts',(90.4430005297902,-1.71947262347024,-0.527745396103237));
#20964=CARTESIAN_POINT('Ctrl Pts',(90.4430005297902,-1.72885247363129,-0.459849352294044));
#20965=CARTESIAN_POINT('Ctrl Pts',(90.4430005297902,-1.73338742826376,-0.427023083951613));
#20966=CARTESIAN_POINT('Ctrl Pts',(90.4430005297902,-1.7369766488472,-0.394030018132786));
#20967=CARTESIAN_POINT('Ctrl Pts',(90.4430005297902,-1.73962237473193,-0.360911589357311));
#20968=CARTESIAN_POINT('',(90.3498698986824,-0.176530238082943,-2.19735656904503));
#20969=CARTESIAN_POINT('Ctrl Pts',(90.4430005297901,1.42252785196811,-1.68345790276294));
#20970=CARTESIAN_POINT('Ctrl Pts',(90.4119569860875,0.984711319553738,-2.05341441334118));
#20971=CARTESIAN_POINT('Ctrl Pts',(90.380913442385,0.394220067868452,-2.23807424546201));
#20972=CARTESIAN_POINT('Ctrl Pts',(90.3498698986824,-0.175612058744845,
-2.19751079506226));
#20973=CARTESIAN_POINT('',(90.3498698986825,-1.48890580190326,0.968619417293912));
#20974=CARTESIAN_POINT('Ctrl Pts',(90.3498698986825,-0.181591443149779,
-2.19650644155094));
#20975=CARTESIAN_POINT('Ctrl Pts',(90.3498698986824,-0.257547497917166,
-2.18363784310906));
#20976=CARTESIAN_POINT('Ctrl Pts',(90.3498698986824,-0.332599118530171,
-2.16671926797206));
#20977=CARTESIAN_POINT('Ctrl Pts',(90.3498698986824,-0.406428811432396,
-2.14565653022378));
#20978=CARTESIAN_POINT('Ctrl Pts',(90.3498698986824,-0.449282745765007,
-2.13343080985508));
#20979=CARTESIAN_POINT('Ctrl Pts',(90.3498698986825,-0.491724687026791,
-2.11980798846392));
#20980=CARTESIAN_POINT('Ctrl Pts',(90.3498698986825,-0.533688867832712,
-2.1047624027297));
#20981=CARTESIAN_POINT('Ctrl Pts',(90.3498698986825,-0.572294897306728,
-2.09092082843577));
#20982=CARTESIAN_POINT('Ctrl Pts',(90.3498698986825,-0.610496552067541,
-2.07587494667674));
#20983=CARTESIAN_POINT('Ctrl Pts',(90.3498698986825,-0.648253856041703,
-2.05966215463177));
#20984=CARTESIAN_POINT('Ctrl Pts',(90.3498698986825,-0.670857500514949,
-2.0499562660028));
#20985=CARTESIAN_POINT('Ctrl Pts',(90.3498698986824,-0.693301845759939,
-2.03983211447534));
#20986=CARTESIAN_POINT('Ctrl Pts',(90.3498698986824,-0.715577834954399,
-2.02929728759008));
#20987=CARTESIAN_POINT('Ctrl Pts',(90.3498698986824,-0.727802722918561,
-2.0235158573124));
#20988=CARTESIAN_POINT('Ctrl Pts',(90.3498698986825,-0.739974677490576,
-2.01761172654651));
#20989=CARTESIAN_POINT('Ctrl Pts',(90.3498698986825,-0.752084605070809,
-2.01159021316281));
#20990=CARTESIAN_POINT('Ctrl Pts',(90.3498698986825,-0.821813208959802,
-1.97691851766653));
#20991=CARTESIAN_POINT('Ctrl Pts',(90.3498698986824,-0.889562996748929,
-1.93832331975832));
#20992=CARTESIAN_POINT('Ctrl Pts',(90.3498698986824,-0.955077779448591,
-1.89609020462415));
#20993=CARTESIAN_POINT('Ctrl Pts',(90.3498698986824,-1.00782120597658,-1.86208995134789));
#20994=CARTESIAN_POINT('Ctrl Pts',(90.3498698986824,-1.05911566372965,-1.82573079165565));
#20995=CARTESIAN_POINT('Ctrl Pts',(90.3498698986824,-1.10880929161884,-1.78714529169387));
#20996=CARTESIAN_POINT('Ctrl Pts',(90.3498698986824,-1.1354927483652,-1.76642644778973));
#20997=CARTESIAN_POINT('Ctrl Pts',(90.3498698986825,-1.16171434281069,-1.74506547534868));
#20998=CARTESIAN_POINT('Ctrl Pts',(90.3498698986825,-1.18744825102447,-1.72308164576251));
#20999=CARTESIAN_POINT('Ctrl Pts',(90.3498698986825,-1.19640383196496,-1.7154311185435));
#21000=CARTESIAN_POINT('Ctrl Pts',(90.3498698986825,-1.20529911666185,-1.70770612424302));
#21001=CARTESIAN_POINT('Ctrl Pts',(90.3498698986825,-1.2141260236274,-1.69991389128878));
#21002=CARTESIAN_POINT('Ctrl Pts',(90.3498698986825,-1.27138360827367,-1.64936793677692));
#21003=CARTESIAN_POINT('Ctrl Pts',(90.3498698986825,-1.32585220394147,-1.59592345892405));
#21004=CARTESIAN_POINT('Ctrl Pts',(90.3498698986825,-1.37729079287515,-1.5398445336278));
#21005=CARTESIAN_POINT('Ctrl Pts',(90.3498698986825,-1.42791166624659,-1.48465709098842));
#21006=CARTESIAN_POINT('Ctrl Pts',(90.3498698986825,-1.47559858119264,-1.42691740718162));
#21007=CARTESIAN_POINT('Ctrl Pts',(90.3498698986825,-1.52007933169953,-1.3668518276762));
#21008=CARTESIAN_POINT('Ctrl Pts',(90.3498698986825,-1.55818476635096,-1.31539529898545));
#21009=CARTESIAN_POINT('Ctrl Pts',(90.3498698986825,-1.59393674881727,-1.26223114492617));
#21010=CARTESIAN_POINT('Ctrl Pts',(90.3498698986825,-1.62713471283202,-1.20749362086064));
#21011=CARTESIAN_POINT('Ctrl Pts',(90.3498698986825,-1.64205050302996,-1.18290014203907));
#21012=CARTESIAN_POINT('Ctrl Pts',(90.3498698986825,-1.65645032490888,-1.15798898503546));
#21013=CARTESIAN_POINT('Ctrl Pts',(90.3498698986825,-1.67031397481906,-1.13277214815258));
#21014=CARTESIAN_POINT('Ctrl Pts',(90.3498698986825,-1.6764049122983,-1.12169323474428));
#21015=CARTESIAN_POINT('Ctrl Pts',(90.3498698986825,-1.68239233832552,-1.11055531714204));
#21016=CARTESIAN_POINT('Ctrl Pts',(90.3498698986825,-1.68827445817782,-1.09935941317281));
#21017=CARTESIAN_POINT('Ctrl Pts',(90.3498698986825,-1.69384736498092,-1.08875205885776));
#21018=CARTESIAN_POINT('Ctrl Pts',(90.3498698986825,-1.69932144666419,-1.07810081173515));
#21019=CARTESIAN_POINT('Ctrl Pts',(90.3498698986825,-1.70469477757153,-1.06740844245854));
#21020=CARTESIAN_POINT('Ctrl Pts',(90.3498698986825,-1.73697093002357,-1.00318225821703));
#21021=CARTESIAN_POINT('Ctrl Pts',(90.3498698986825,-1.76562679489482,-0.93745261723568));
#21022=CARTESIAN_POINT('Ctrl Pts',(90.3498698986825,-1.79041933775187,-0.870427041020484));
#21023=CARTESIAN_POINT('Ctrl Pts',(90.3498698986825,-1.80872633921582,-0.82093484778445));
#21024=CARTESIAN_POINT('Ctrl Pts',(90.3498698986825,-1.82492598564089,-0.770735606075043));
#21025=CARTESIAN_POINT('Ctrl Pts',(90.3498698986825,-1.83890236465801,-0.719909707048012));
#21026=CARTESIAN_POINT('Ctrl Pts',(90.3498698986825,-1.85827904310889,-0.649445311283019));
#21027=CARTESIAN_POINT('Ctrl Pts',(90.3498698986825,-1.87338410188164,-0.577775460624741));
#21028=CARTESIAN_POINT('Ctrl Pts',(90.3498698986825,-1.88426075716109,-0.505262831297774));
#21029=CARTESIAN_POINT('Ctrl Pts',(90.3498698986825,-1.88955943874573,-0.469937510802043));
#21030=CARTESIAN_POINT('Ctrl Pts',(90.3498698986825,-1.89385383550167,-0.434412328240286));
#21031=CARTESIAN_POINT('Ctrl Pts',(90.3498698986825,-1.8971447051508,-0.398730679953565));
#21032=CARTESIAN_POINT('Ctrl Pts',(90.3498698986825,-1.89872539720831,-0.381591837015542));
#21033=CARTESIAN_POINT('Ctrl Pts',(90.3498698986825,-1.90007477485771,-0.364410850502332));
#21034=CARTESIAN_POINT('Ctrl Pts',(90.3498698986825,-1.90119093547224,-0.347226454365849));
#21035=CARTESIAN_POINT('Ctrl Pts',(90.3498698986825,-1.90580822290102,-0.276138749586064));
#21036=CARTESIAN_POINT('Ctrl Pts',(90.3498698986825,-1.90644977781024,-0.204903322611939));
#21037=CARTESIAN_POINT('Ctrl Pts',(90.3498698986825,-1.90320526373546,-0.133853409269437));
#21038=CARTESIAN_POINT('Ctrl Pts',(90.3498698986825,-1.89997246403425,-0.0630600228543288));
#21039=CARTESIAN_POINT('Ctrl Pts',(90.3498698986825,-1.89288121916131,0.00755020257709174));
#21040=CARTESIAN_POINT('Ctrl Pts',(90.3498698986825,-1.88197092147295,0.0776346496953351));
#21041=CARTESIAN_POINT('Ctrl Pts',(90.3498698986825,-1.87114890638586,0.147151996127894));
#21042=CARTESIAN_POINT('Ctrl Pts',(90.3498698986825,-1.85656900401952,0.216152960759292));
#21043=CARTESIAN_POINT('Ctrl Pts',(90.3498698986825,-1.83822688126874,0.284276007636229));
#21044=CARTESIAN_POINT('Ctrl Pts',(90.3498698986825,-1.83385334097406,0.300519432378364));
#21045=CARTESIAN_POINT('Ctrl Pts',(90.3498698986825,-1.82926572255453,0.316712786174135));
#21046=CARTESIAN_POINT('Ctrl Pts',(90.3498698986825,-1.82446364132743,0.332850848989152));
#21047=CARTESIAN_POINT('Ctrl Pts',(90.3498698986825,-1.82014892639808,0.347351049478418));
#21048=CARTESIAN_POINT('Ctrl Pts',(90.3498698986825,-1.81565974396159,0.361810316796932));
#21049=CARTESIAN_POINT('Ctrl Pts',(90.3498698986825,-1.81100440526727,0.376199140206946));
#21050=CARTESIAN_POINT('Ctrl Pts',(90.3498698986825,-1.78985030303721,0.441582705479499));
#21051=CARTESIAN_POINT('Ctrl Pts',(90.3498698986825,-1.7652408840571,0.505614703301049));
#21052=CARTESIAN_POINT('Ctrl Pts',(90.3498698986825,-1.73722113972244,0.567982945175986));
#21053=CARTESIAN_POINT('Ctrl Pts',(90.3498698986825,-1.70966066292315,0.629328918311083));
#21054=CARTESIAN_POINT('Ctrl Pts',(90.3498698986825,-1.67880028902505,0.689065998029432));
#21055=CARTESIAN_POINT('Ctrl Pts',(90.3498698986825,-1.64464358716772,0.746866444995096));
#21056=CARTESIAN_POINT('Ctrl Pts',(90.3498698986825,-1.61157576824413,0.802824269083222));
#21057=CARTESIAN_POINT('Ctrl Pts',(90.3498698986825,-1.57541798153181,0.856967478920098));
#21058=CARTESIAN_POINT('Ctrl Pts',(90.3498698986825,-1.5361431033198,0.90896063293066));
#21059=CARTESIAN_POINT('Ctrl Pts',(90.3498698986825,-1.52086991362194,0.929179697644421));
#21060=CARTESIAN_POINT('Ctrl Pts',(90.3498698986825,-1.50512503817006,0.949073159038998));
#21061=CARTESIAN_POINT('Ctrl Pts',(90.3498698986825,-1.48890580190332,0.968619417293828));
#21062=CARTESIAN_POINT('Ctrl Pts',(90.3498698986825,-1.48890580190326,0.968619417293918));
#21063=CARTESIAN_POINT('Ctrl Pts',(90.3541932148582,-1.52398815970758,0.914692843918768));
#21064=CARTESIAN_POINT('Ctrl Pts',(90.3585165310339,-1.5561759881181,0.858798217428194));
#21065=CARTESIAN_POINT('Ctrl Pts',(90.3628398472097,-1.58525053530777,0.801276982576202));
#21066=CARTESIAN_POINT('Ctrl Pts',(90.367160134058,-1.61430471009857,0.743796052583733));
#21067=CARTESIAN_POINT('Ctrl Pts',(90.3714804209064,-1.64024971073537,0.684691215118076));
#21068=CARTESIAN_POINT('Ctrl Pts',(90.3758007077547,-1.66291209690492,0.624329576800017));
#21069=CARTESIAN_POINT('Ctrl Pts',(90.3801194360565,-1.68556630760244,0.563989713986172));
#21070=CARTESIAN_POINT('Ctrl Pts',(90.3844381643583,-1.70494008238903,0.502394412118546));
#21071=CARTESIAN_POINT('Ctrl Pts',(90.3887568926601,-1.72090833927923,0.439930165252616));
#21072=CARTESIAN_POINT('Ctrl Pts',(90.3932660508206,-1.73758069994543,0.374711622010738));
#21073=CARTESIAN_POINT('Ctrl Pts',(90.3977752089812,-1.75054004309615,0.308546266800645));
#21074=CARTESIAN_POINT('Ctrl Pts',(90.4022843671418,-1.75970278433496,0.241888762251942));
#21075=CARTESIAN_POINT('Ctrl Pts',(90.4066067777444,-1.76848604907515,0.177991889677299));
#21076=CARTESIAN_POINT('Ctrl Pts',(90.410929188347,-1.77378100929878,0.113643352831989));
#21077=CARTESIAN_POINT('Ctrl Pts',(90.4152515989496,-1.77556711921805,0.0492490370638697));
#21078=CARTESIAN_POINT('Ctrl Pts',(90.419576346189,-1.7773541946842,-0.0151800894010165));
#21079=CARTESIAN_POINT('Ctrl Pts',(90.4239010934283,-1.77562865381725,-0.0796545509734151));
#21080=CARTESIAN_POINT('Ctrl Pts',(90.4282258406677,-1.7704220529785,-0.143770013658602));
#21081=CARTESIAN_POINT('Ctrl Pts',(90.4325566335551,-1.76520817373151,-0.207975104591915));
#21082=CARTESIAN_POINT('Ctrl Pts',(90.4368874264424,-1.75650359197293,-0.271819707280591));
#21083=CARTESIAN_POINT('Ctrl Pts',(90.4412182193298,-1.7443913320854,-0.334907364871723));
#21084=CARTESIAN_POINT('Ctrl Pts',(90.4417677430822,-1.74285443695412,-0.342912403955771));
#21085=CARTESIAN_POINT('Ctrl Pts',(90.4423172668345,-1.74126274301271,-0.350905274149106));
#21086=CARTESIAN_POINT('Ctrl Pts',(90.4428667905869,-1.7396164773305,-0.358885182614482));
#21087=CARTESIAN_POINT('Origin',(88.3562164250559,0.,0.));
#21088=CARTESIAN_POINT('',(90.4430005297901,-0.906280710947669,1.52765157528285));
#21089=CARTESIAN_POINT('Origin',(90.4430005297901,0.,0.));
#21090=CARTESIAN_POINT('',(90.3500036506772,0.430448222620968,1.72330449722109));
#21091=CARTESIAN_POINT('Origin',(90.3498698986825,0.,0.));
#21092=CARTESIAN_POINT('Ctrl Pts',(90.3500036506772,0.430448222620968,1.72330449722109));
#21093=CARTESIAN_POINT('Ctrl Pts',(90.3543334549293,0.368162530036945,1.73886226180115));
#21094=CARTESIAN_POINT('Ctrl Pts',(90.3586632591815,0.304931496232834,1.75106421633573));
#21095=CARTESIAN_POINT('Ctrl Pts',(90.3629930634336,0.241145549042035,1.75980478652526));
#21096=CARTESIAN_POINT('Ctrl Pts',(90.3673177204846,0.177435429551993,1.76853496606653));
#21097=CARTESIAN_POINT('Ctrl Pts',(90.3716423775356,0.113172191084751,1.77381185872338));
#21098=CARTESIAN_POINT('Ctrl Pts',(90.3759670345866,0.0487574122840727,
1.77558068733791));
#21099=CARTESIAN_POINT('Ctrl Pts',(90.3802880212225,-0.0156026965218813,
1.77734801471541));
#21100=CARTESIAN_POINT('Ctrl Pts',(90.3846090078583,-0.0801135989579022,
1.77561317440503));
#21101=CARTESIAN_POINT('Ctrl Pts',(90.3889299944942,-0.144369453052096,
1.77037327237095));
#21102=CARTESIAN_POINT('Ctrl Pts',(90.3934358724355,-0.211374759932788,
1.76490915943109));
#21103=CARTESIAN_POINT('Ctrl Pts',(90.3979417503768,-0.278102135650947,
1.75563321327166));
#21104=CARTESIAN_POINT('Ctrl Pts',(90.4024476283182,-0.34409391660832,1.74260249025793));
#21105=CARTESIAN_POINT('Ctrl Pts',(90.4067670445942,-0.407354834117631,
1.73011100295907));
#21106=CARTESIAN_POINT('Ctrl Pts',(90.4110864608703,-0.469939331470611,
1.71416954088058));
#21107=CARTESIAN_POINT('Ctrl Pts',(90.4154058771463,-0.531454112471102,
1.6948807004735));
#21108=CARTESIAN_POINT('Ctrl Pts',(90.4197258212459,-0.592976410447589,
1.67558950301097));
#21109=CARTESIAN_POINT('Ctrl Pts',(90.4240457653455,-0.653428264985323,
1.65295027247733));
#21110=CARTESIAN_POINT('Ctrl Pts',(90.4283657094451,-0.712433136210315,
1.62711495873203));
#21111=CARTESIAN_POINT('Ctrl Pts',(90.4326892060825,-0.771486530525676,
1.60125839912622));
#21112=CARTESIAN_POINT('Ctrl Pts',(90.4370127027199,-0.829090122470763,
1.57220072507932));
#21113=CARTESIAN_POINT('Ctrl Pts',(90.4413361993573,-0.884890167582664,
1.54014072532854));
#21114=CARTESIAN_POINT('Ctrl Pts',(90.4418909761683,-0.89205024510147,1.5360268920331));
#21115=CARTESIAN_POINT('Ctrl Pts',(90.4424457529792,-0.899180664056975,
1.53186368467218));
#21116=CARTESIAN_POINT('Ctrl Pts',(90.4430005297901,-0.90628071094767,1.52765157528285));
#21117=CARTESIAN_POINT('Ctrl Pts',(90.1025143645163,1.30770975493414,-1.2010560632029));
#21118=CARTESIAN_POINT('Ctrl Pts',(90.1403023877111,1.68793071858886,-0.787071505416501));
#21119=CARTESIAN_POINT('Ctrl Pts',(90.2158784341009,2.0214346950512,0.423355288987036));
#21120=CARTESIAN_POINT('Ctrl Pts',(90.3292456386917,0.830626863199002,1.8909219215733));
#21121=CARTESIAN_POINT('Ctrl Pts',(90.4048248200878,-0.422610284094226,
1.81385139676035));
#21122=CARTESIAN_POINT('Ctrl Pts',(90.442615978289,-0.906052876477412,1.52699333780199));
#21123=CARTESIAN_POINT('Ctrl Pts',(90.1849662092383,1.41289023394354,-1.29765827295793));
#21124=CARTESIAN_POINT('Ctrl Pts',(90.2227542324332,1.82369277193898,-0.850376499236438));
#21125=CARTESIAN_POINT('Ctrl Pts',(90.2983302788229,2.18402082604052,0.457406202745833));
#21126=CARTESIAN_POINT('Ctrl Pts',(90.4116974834138,0.897435060522396,2.04301077212292));
#21127=CARTESIAN_POINT('Ctrl Pts',(90.4872766648098,-0.45660127632136,1.95974138346671));
#21128=CARTESIAN_POINT('Ctrl Pts',(90.525067823011,-0.978927667841591,1.64981102736054));
#21129=CARTESIAN_POINT('Ctrl Pts',(90.2674180539604,1.51807071295294,-1.39426048271296));
#21130=CARTESIAN_POINT('Ctrl Pts',(90.3052060771553,1.95945482528912,-0.913681493056375));
#21131=CARTESIAN_POINT('Ctrl Pts',(90.3807821235449,2.34660695702982,0.491457116504633));
#21132=CARTESIAN_POINT('Ctrl Pts',(90.4941493281359,0.964243257845793,2.19509962267253));
#21133=CARTESIAN_POINT('Ctrl Pts',(90.5697285095319,-0.490592268548493,
2.10563137017308));
#21134=CARTESIAN_POINT('Ctrl Pts',(90.607519667733,-1.05180245920577,1.77262871691909));
#21135=CARTESIAN_POINT('Ctrl Pts',(90.3498698986825,1.62325119196233,-1.49086269246798));
#21136=CARTESIAN_POINT('Ctrl Pts',(90.3876579218773,2.09521687863925,-0.976986486876311));
#21137=CARTESIAN_POINT('Ctrl Pts',(90.463233968267,2.50919308801913,0.52550803026343));
#21138=CARTESIAN_POINT('Ctrl Pts',(90.5766011728579,1.03105145516918,2.34718847322216));
#21139=CARTESIAN_POINT('Ctrl Pts',(90.6521803542539,-0.524583260775627,
2.25152135687945));
#21140=CARTESIAN_POINT('Ctrl Pts',(90.6899715124551,-1.12467725056995,1.89544640647765));
#21141=CARTESIAN_POINT('',(90.4430005297901,2.20288941995875,0.0846757462792571));
#21142=CARTESIAN_POINT('Ctrl Pts',(90.4430005297901,-0.906280710947681,
1.52765157528286));
#21143=CARTESIAN_POINT('Ctrl Pts',(90.4430005297901,-0.85427776061733,1.56729260000203));
#21144=CARTESIAN_POINT('Ctrl Pts',(90.4430005297901,-0.800108744347126,
1.60369925010846));
#21145=CARTESIAN_POINT('Ctrl Pts',(90.4430005297901,-0.74412579004436,1.6369238377391));
#21146=CARTESIAN_POINT('Ctrl Pts',(90.4430005297901,-0.686154010778423,
1.67132874695323));
#21147=CARTESIAN_POINT('Ctrl Pts',(90.4430005297901,-0.626236599135055,
1.70232196502649));
#21148=CARTESIAN_POINT('Ctrl Pts',(90.4430005297901,-0.56471892524639,1.72992757470838));
#21149=CARTESIAN_POINT('Ctrl Pts',(90.4430005297901,-0.512092172819651,
1.75354344791171));
#21150=CARTESIAN_POINT('Ctrl Pts',(90.4430005297901,-0.458293231183982,
1.77467969048158));
#21151=CARTESIAN_POINT('Ctrl Pts',(90.4430005297901,-0.403518249784151,
1.7933288252926));
#21152=CARTESIAN_POINT('Ctrl Pts',(90.4430005297901,-0.378653325916346,
1.80179453911716));
#21153=CARTESIAN_POINT('Ctrl Pts',(90.4430005297901,-0.353587059186379,
1.80974744290714));
#21154=CARTESIAN_POINT('Ctrl Pts',(90.4430005297901,-0.328336895404222,
1.81718529672686));
#21155=CARTESIAN_POINT('Ctrl Pts',(90.4430005297901,-0.315371182046074,
1.82100456227533));
#21156=CARTESIAN_POINT('Ctrl Pts',(90.4430005297901,-0.302356972411376,
1.82468800737921));
#21157=CARTESIAN_POINT('Ctrl Pts',(90.4430005297901,-0.289296585325212,
1.82823522504612));
#21158=CARTESIAN_POINT('Ctrl Pts',(90.4430005297901,-0.27797522962883,1.83131011958597));
#21159=CARTESIAN_POINT('Ctrl Pts',(90.4430005297901,-0.266619082046209,
1.83428258023669));
#21160=CARTESIAN_POINT('Ctrl Pts',(90.4430005297901,-0.255244023393882,
1.83714894810173));
#21161=CARTESIAN_POINT('Ctrl Pts',(90.4430005297901,-0.186861532625867,
1.85438045257656));
#21162=CARTESIAN_POINT('Ctrl Pts',(90.4430005297901,-0.117671879173756,
1.86781631415273));
#21163=CARTESIAN_POINT('Ctrl Pts',(90.4430005297901,-0.0480425183926124,
1.87748511039214));
#21164=CARTESIAN_POINT('Ctrl Pts',(90.4430005297901,0.022546181818848,1.88728712137563));
#21165=CARTESIAN_POINT('Ctrl Pts',(90.4430005297901,0.0935877174917611,
1.89321794763905));
#21166=CARTESIAN_POINT('Ctrl Pts',(90.4430005297901,0.164729041340744,1.89526279950741));
#21167=CARTESIAN_POINT('Ctrl Pts',(90.4430005297901,0.235739474401595,1.89730388911415));
#21168=CARTESIAN_POINT('Ctrl Pts',(90.4430005297901,0.306850371500938,1.895473589152));
#21169=CARTESIAN_POINT('Ctrl Pts',(90.4430005297901,0.377725173679166,1.88970801775623));
#21170=CARTESIAN_POINT('Ctrl Pts',(90.4430005297901,0.387086066100972,1.88894652154139));
#21171=CARTESIAN_POINT('Ctrl Pts',(90.4430005297901,0.396442847540759,1.88811630351686));
#21172=CARTESIAN_POINT('Ctrl Pts',(90.4430005297901,0.405794746349183,1.88721714781832));
#21173=CARTESIAN_POINT('Ctrl Pts',(90.4430005297901,0.419068452783981,1.88594092263388));
#21174=CARTESIAN_POINT('Ctrl Pts',(90.4430005297901,0.432332323108796,1.88452581977723));
#21175=CARTESIAN_POINT('Ctrl Pts',(90.4430005297901,0.445584146956699,1.88297116443227));
#21176=CARTESIAN_POINT('Ctrl Pts',(90.4430005297901,0.458728559964045,1.88142911013296));
#21177=CARTESIAN_POINT('Ctrl Pts',(90.4430005297901,0.471853391141756,1.87975060439523));
#21178=CARTESIAN_POINT('Ctrl Pts',(90.4430005297901,0.484948310227803,1.87793672161782));
#21179=CARTESIAN_POINT('Ctrl Pts',(90.4430005297901,0.557788263474285,1.8678470726606));
#21180=CARTESIAN_POINT('Ctrl Pts',(90.4430005297901,0.629779464650554,1.85356363281225));
#21181=CARTESIAN_POINT('Ctrl Pts',(90.4430005297901,0.700551912386963,1.8350809107756));
#21182=CARTESIAN_POINT('Ctrl Pts',(90.4430005297901,0.732380673074809,1.82676860626473));
#21183=CARTESIAN_POINT('Ctrl Pts',(90.4430005297901,0.763963163282869,1.81760628974153));
#21184=CARTESIAN_POINT('Ctrl Pts',(90.4430005297901,0.795266463078774,1.80759010215849));
#21185=CARTESIAN_POINT('Ctrl Pts',(90.4430005297901,0.862738051477974,1.78600106552856));
#21186=CARTESIAN_POINT('Ctrl Pts',(90.4430005297901,0.928913182268453,1.76044866334016));
#21187=CARTESIAN_POINT('Ctrl Pts',(90.4430005297901,0.993607519094083,1.73121543301718));
#21188=CARTESIAN_POINT('Ctrl Pts',(90.4430005297901,1.05227136538682,1.70470718184011));
#21189=CARTESIAN_POINT('Ctrl Pts',(90.4430005297901,1.10971794982988,1.67517139596582));
#21190=CARTESIAN_POINT('Ctrl Pts',(90.4430005297901,1.16580106122499,1.64278422184807));
#21191=CARTESIAN_POINT('Ctrl Pts',(90.4430005297901,1.17624228698311,1.63675456714064));
#21192=CARTESIAN_POINT('Ctrl Pts',(90.4430005297901,1.18662850495695,1.63063043366676));
#21193=CARTESIAN_POINT('Ctrl Pts',(90.4430005297901,1.19695660054927,1.62441474165913));
#21194=CARTESIAN_POINT('Ctrl Pts',(90.4430005297901,1.2599916564761,1.58647875531759));
#21195=CARTESIAN_POINT('Ctrl Pts',(90.4430005297901,1.32088999312167,1.54512054404452));
#21196=CARTESIAN_POINT('Ctrl Pts',(90.4430005297901,1.37946364278683,1.50067032138885));
#21197=CARTESIAN_POINT('Ctrl Pts',(90.4430005297901,1.43980234043913,1.45488064359463));
#21198=CARTESIAN_POINT('Ctrl Pts',(90.4430005297901,1.49767496244285,1.4058094546661));
#21199=CARTESIAN_POINT('Ctrl Pts',(90.4430005297901,1.55286316604442,1.35376300242344));
#21200=CARTESIAN_POINT('Ctrl Pts',(90.4430005297901,1.60805136964599,1.30171655018078));
#21201=CARTESIAN_POINT('Ctrl Pts',(90.4430005297901,1.66055597518215,1.24669418492708));
#21202=CARTESIAN_POINT('Ctrl Pts',(90.4430005297901,1.7101335714528,1.18895618401779));
#21203=CARTESIAN_POINT('Ctrl Pts',(90.4430005297901,1.72296507476097,1.17401263278892));
#21204=CARTESIAN_POINT('Ctrl Pts',(90.4430005297901,1.73560034241774,1.15888696127209));
#21205=CARTESIAN_POINT('Ctrl Pts',(90.4430005297901,1.74803477487698,1.14358326375263));
#21206=CARTESIAN_POINT('Ctrl Pts',(90.4430005297901,1.76083174777711,1.12783336900912));
#21207=CARTESIAN_POINT('Ctrl Pts',(90.4430005297901,1.77341879728596,1.11189092493476));
#21208=CARTESIAN_POINT('Ctrl Pts',(90.4430005297901,1.78576841317895,1.09579034652114));
#21209=CARTESIAN_POINT('Ctrl Pts',(90.4430005297901,1.83344349969373,1.0336348531472));
#21210=CARTESIAN_POINT('Ctrl Pts',(90.4430005297901,1.87765235973484,0.96904318707649));
#21211=CARTESIAN_POINT('Ctrl Pts',(90.4430005297901,1.91815905619862,0.902327591878008));
#21212=CARTESIAN_POINT('Ctrl Pts',(90.4430005297901,1.95747515212669,0.837572947098043));
#21213=CARTESIAN_POINT('Ctrl Pts',(90.4430005297901,1.9933041333804,0.770816566127668));
#21214=CARTESIAN_POINT('Ctrl Pts',(90.4430005297901,2.025399552996,0.702308430193668));
#21215=CARTESIAN_POINT('Ctrl Pts',(90.4430005297901,2.03357309269835,0.684861891849661));
#21216=CARTESIAN_POINT('Ctrl Pts',(90.4430005297901,2.04150431230283,0.667301596050374));
#21217=CARTESIAN_POINT('Ctrl Pts',(90.4430005297901,2.04918873720808,0.649631385046058));
#21218=CARTESIAN_POINT('Ctrl Pts',(90.4430005297901,2.05507993245338,0.636084676693029));
#21219=CARTESIAN_POINT('Ctrl Pts',(90.4430005297901,2.06082532051455,0.622474881182825));
#21220=CARTESIAN_POINT('Ctrl Pts',(90.4430005297901,2.06641865115953,0.608814817998374));
#21221=CARTESIAN_POINT('Ctrl Pts',(90.4430005297901,2.08828602816888,0.555410188344606));
#21222=CARTESIAN_POINT('Ctrl Pts',(90.4430005297901,2.10785002137055,0.501192775045439));
#21223=CARTESIAN_POINT('Ctrl Pts',(90.4430005297901,2.12501355371717,0.446278571766083));
#21224=CARTESIAN_POINT('Ctrl Pts',(90.4430005297901,2.14793295023584,0.372948654937288));
#21225=CARTESIAN_POINT('Ctrl Pts',(90.4430005297901,2.16657429829944,0.298376904669313));
#21226=CARTESIAN_POINT('Ctrl Pts',(90.4430005297901,2.181072682182,0.222889057477663));
#21227=CARTESIAN_POINT('Ctrl Pts',(90.4430005297901,2.18985901388012,0.177141802474964));
#21228=CARTESIAN_POINT('Ctrl Pts',(90.4430005297901,2.19712286143767,0.131057562767499));
#21229=CARTESIAN_POINT('Ctrl Pts',(90.4430005297901,2.20288574446881,0.0847053108012298));
#21230=CARTESIAN_POINT('',(90.3498698986825,1.62325119196235,-1.49086269246796));
#21231=CARTESIAN_POINT('Ctrl Pts',(90.3498698986825,0.432473260079398,1.72322635770741));
#21232=CARTESIAN_POINT('Ctrl Pts',(90.3498698986825,0.500689037073845,1.71492876273113));
#21233=CARTESIAN_POINT('Ctrl Pts',(90.3498698986825,0.568201159921543,1.70262361322679));
#21234=CARTESIAN_POINT('Ctrl Pts',(90.3498698986825,0.634646799814703,1.68629351059737));
#21235=CARTESIAN_POINT('Ctrl Pts',(90.3498698986825,0.666771821708387,1.67839826110711));
#21236=CARTESIAN_POINT('Ctrl Pts',(90.3498698986825,0.698647807968656,1.66956143909893));
#21237=CARTESIAN_POINT('Ctrl Pts',(90.3498698986825,0.730234584403302,1.65977677709576));
#21238=CARTESIAN_POINT('Ctrl Pts',(90.3498698986825,0.766337183991592,1.64859324479901));
#21239=CARTESIAN_POINT('Ctrl Pts',(90.3498698986825,0.80206203264144,1.63617162624099));
#21240=CARTESIAN_POINT('Ctrl Pts',(90.3498698986825,0.83737540599978,1.62256200026643));
#21241=CARTESIAN_POINT('Ctrl Pts',(90.3498698986825,0.852643420161424,1.6166777716484));
#21242=CARTESIAN_POINT('Ctrl Pts',(90.3498698986825,0.867834507669581,1.61057139499706));
#21243=CARTESIAN_POINT('Ctrl Pts',(90.3498698986825,0.882945892123966,1.60424660726946));
#21244=CARTESIAN_POINT('Ctrl Pts',(90.3498698986825,0.894457590187188,1.59942844869149));
#21245=CARTESIAN_POINT('Ctrl Pts',(90.3498698986825,0.905920948354237,1.59448434130904));
#21246=CARTESIAN_POINT('Ctrl Pts',(90.3498698986825,0.917326683635243,1.58941980305413));
#21247=CARTESIAN_POINT('Ctrl Pts',(90.3498698986825,0.979664976032291,1.56173945989233));
#21248=CARTESIAN_POINT('Ctrl Pts',(90.3498698986825,1.04035172112798,1.53043727359164));
#21249=CARTESIAN_POINT('Ctrl Pts',(90.3498698986825,1.09919843954761,1.49582959806102));
#21250=CARTESIAN_POINT('Ctrl Pts',(90.3498698986825,1.15010544629707,1.46589125622763));
#21251=CARTESIAN_POINT('Ctrl Pts',(90.3498698986825,1.19963574840911,1.43347809868508));
#21252=CARTESIAN_POINT('Ctrl Pts',(90.3498698986825,1.24766201189903,1.39876400501926));
#21253=CARTESIAN_POINT('Ctrl Pts',(90.3498698986825,1.26296034952527,1.38770614028657));
#21254=CARTESIAN_POINT('Ctrl Pts',(90.3498698986825,1.27810601388692,1.37641460218754));
#21255=CARTESIAN_POINT('Ctrl Pts',(90.3498698986825,1.2930946896096,1.364894468081));
#21256=CARTESIAN_POINT('Ctrl Pts',(90.3498698986825,1.30640467453454,1.35466455757203));
#21257=CARTESIAN_POINT('Ctrl Pts',(90.3498698986825,1.31959368966207,1.34425192002827));
#21258=CARTESIAN_POINT('Ctrl Pts',(90.3498698986825,1.33263794396078,1.33367724437742));
#21259=CARTESIAN_POINT('Ctrl Pts',(90.3498698986825,1.387780351554,1.28897456827561));
#21260=CARTESIAN_POINT('Ctrl Pts',(90.3498698986825,1.44040951214014,1.24132658213606));
#21261=CARTESIAN_POINT('Ctrl Pts',(90.3498698986825,1.49033018857133,1.19105566693961));
#21262=CARTESIAN_POINT('Ctrl Pts',(90.3498698986825,1.54132495681077,1.13970312420791));
#21263=CARTESIAN_POINT('Ctrl Pts',(90.3498698986825,1.58949432646132,1.08561309737197));
#21264=CARTESIAN_POINT('Ctrl Pts',(90.3498698986825,1.63461237100243,1.02907775284));
#21265=CARTESIAN_POINT('Ctrl Pts',(90.3498698986825,1.67109719585865,0.983360298450885));
#21266=CARTESIAN_POINT('Ctrl Pts',(90.3498698986825,1.70558655723711,0.936042670436095));
#21267=CARTESIAN_POINT('Ctrl Pts',(90.3498698986825,1.73794656373636,0.887259053299169));
#21268=CARTESIAN_POINT('Ctrl Pts',(90.3498698986825,1.75291021222756,0.864700933634306));
#21269=CARTESIAN_POINT('Ctrl Pts',(90.3498698986825,1.76741833878176,0.841829120502182));
#21270=CARTESIAN_POINT('Ctrl Pts',(90.3498698986825,1.78145646826647,0.818655805601395));
#21271=CARTESIAN_POINT('Ctrl Pts',(90.3498698986825,1.7878902939984,0.808035226138496));
#21272=CARTESIAN_POINT('Ctrl Pts',(90.3498698986825,1.7942263747759,0.797349598647959));
#21273=CARTESIAN_POINT('Ctrl Pts',(90.3498698986825,1.80046011156049,0.786605484523132));
#21274=CARTESIAN_POINT('Ctrl Pts',(90.3498698986825,1.83793113462125,0.722022560660496));
#21275=CARTESIAN_POINT('Ctrl Pts',(90.3498698986825,1.87157440109655,0.65556035740974));
#21276=CARTESIAN_POINT('Ctrl Pts',(90.3498698986825,1.90116665684937,0.587535602342418));
#21277=CARTESIAN_POINT('Ctrl Pts',(90.3498698986825,1.926007323006,0.530433492752384));
#21278=CARTESIAN_POINT('Ctrl Pts',(90.3498698986825,1.94799336759589,0.472229235594803));
#21279=CARTESIAN_POINT('Ctrl Pts',(90.3498698986825,1.96697450572884,0.41308845846253));
#21280=CARTESIAN_POINT('Ctrl Pts',(90.3498698986825,1.9890681716311,0.344249774395821));
#21281=CARTESIAN_POINT('Ctrl Pts',(90.3498698986825,2.00709239698971,0.274142320648795));
#21282=CARTESIAN_POINT('Ctrl Pts',(90.3498698986825,2.02116104200378,0.2030743095277));
#21283=CARTESIAN_POINT('Ctrl Pts',(90.3498698986825,2.0284921104876,0.166041286374636));
#21284=CARTESIAN_POINT('Ctrl Pts',(90.3498698986825,2.03474828995425,0.128747041235049));
#21285=CARTESIAN_POINT('Ctrl Pts',(90.3498698986825,2.03994046639292,0.0912332730845004));
#21286=CARTESIAN_POINT('Ctrl Pts',(90.3498698986825,2.04159548143424,0.0792756958951614));
#21287=CARTESIAN_POINT('Ctrl Pts',(90.3498698986825,2.04314268181887,0.0672931065835392));
#21288=CARTESIAN_POINT('Ctrl Pts',(90.3498698986825,2.04458127608794,0.0552958865448529));
#21289=CARTESIAN_POINT('Ctrl Pts',(90.3498698986825,2.05337295176515,-0.0180226785820481));
#21290=CARTESIAN_POINT('Ctrl Pts',(90.3498698986825,2.05809534086584,-0.091727701576409));
#21291=CARTESIAN_POINT('Ctrl Pts',(90.3498698986825,2.05891131036719,-0.165484762986751));
#21292=CARTESIAN_POINT('Ctrl Pts',(90.3498698986825,2.05975504538824,-0.241751603424167));
#21293=CARTESIAN_POINT('Ctrl Pts',(90.3498698986825,2.05642222258532,-0.318074882014285));
#21294=CARTESIAN_POINT('Ctrl Pts',(90.3498698986825,2.04904110315175,-0.394108580285359));
#21295=CARTESIAN_POINT('Ctrl Pts',(90.3498698986825,2.04165998371819,-0.470142278556433));
#21296=CARTESIAN_POINT('Ctrl Pts',(90.3498698986825,2.03023052284998,-0.545887393004193));
#21297=CARTESIAN_POINT('Ctrl Pts',(90.3498698986825,2.01482901135003,-0.621007387284472));
#21298=CARTESIAN_POINT('Ctrl Pts',(90.3498698986825,2.0082558082846,-0.653067810489035));
#21299=CARTESIAN_POINT('Ctrl Pts',(90.3498698986825,2.00095845789534,-0.685014398435952));
#21300=CARTESIAN_POINT('Ctrl Pts',(90.3498698986825,1.99294003791299,-0.716820819516161));
#21301=CARTESIAN_POINT('Ctrl Pts',(90.3498698986825,1.98892248395689,-0.732757127806477));
#21302=CARTESIAN_POINT('Ctrl Pts',(90.3498698986825,1.98472264433956,-0.748662300766753));
#21303=CARTESIAN_POINT('Ctrl Pts',(90.3498698986825,1.98034860459118,-0.764505835419562));
#21304=CARTESIAN_POINT('Ctrl Pts',(90.3498698986825,1.95934426572363,-0.840587213242088));
#21305=CARTESIAN_POINT('Ctrl Pts',(90.3498698986825,1.93430052129626,-0.915360726877347));
#21306=CARTESIAN_POINT('Ctrl Pts',(90.3498698986825,1.9053538503144,-0.988470818961527));
#21307=CARTESIAN_POINT('Ctrl Pts',(90.3498698986825,1.87638204881937,-1.06164438273589));
#21308=CARTESIAN_POINT('Ctrl Pts',(90.3498698986825,1.8435004604713,-1.13315267365001));
#21309=CARTESIAN_POINT('Ctrl Pts',(90.3498698986825,1.80679432960359,-1.202641416107));
#21310=CARTESIAN_POINT('Ctrl Pts',(90.3498698986825,1.77047936629771,-1.27138963535113));
#21311=CARTESIAN_POINT('Ctrl Pts',(90.3498698986825,1.73042077500903,-1.33816212418568));
#21312=CARTESIAN_POINT('Ctrl Pts',(90.3498698986825,1.6866526119066,-1.4026027958059));
#21313=CARTESIAN_POINT('Ctrl Pts',(90.3498698986825,1.66632005262628,-1.43253879683743));
#21314=CARTESIAN_POINT('Ctrl Pts',(90.3498698986825,1.64518626524376,-1.46197129625266));
#21315=CARTESIAN_POINT('Ctrl Pts',(90.3498698986825,1.62325119196239,-1.49086269246791));
#21316=CARTESIAN_POINT('Ctrl Pts',(90.3498698986825,1.62325119196235,-1.49086269246796));
#21317=CARTESIAN_POINT('Ctrl Pts',(90.380913442385,2.01097952971941,-1.06870410630073));
#21318=CARTESIAN_POINT('Ctrl Pts',(90.4119569860876,2.21987663538069,-0.486345711720857));
#21319=CARTESIAN_POINT('Ctrl Pts',(90.4430005297901,2.20288941995875,0.0846757462792571));
#21320=CARTESIAN_POINT('Origin',(90.3498698986825,-2.40291074888303E-16,
0.));
#21321=CARTESIAN_POINT('',(90.3498698986825,-2.69912154532077E-16,2.204));
#21322=CARTESIAN_POINT('Origin',(90.3498698986825,0.,0.));
#21323=CARTESIAN_POINT('Origin',(90.3498698986825,0.,0.));
#21324=CARTESIAN_POINT('Origin',(66.9212607628943,0.,0.));
#21325=CARTESIAN_POINT('',(81.4430005297901,-2.69912154532077E-16,2.204));
#21326=CARTESIAN_POINT('Origin',(81.4430005297901,0.,0.));
#21327=CARTESIAN_POINT('',(66.9212607628943,-2.69912154532077E-16,2.204));
#21328=CARTESIAN_POINT('Origin',(90.4430005297901,0.,0.));
#21329=CARTESIAN_POINT('Ctrl Pts',(82.0295201802136,-1.65306427348725,3.32899555241991));
#21330=CARTESIAN_POINT('Ctrl Pts',(82.0621173237355,-2.19852390520666,3.05813912872495));
#21331=CARTESIAN_POINT('Ctrl Pts',(82.1273116107797,-3.14747075323877,2.24346380767911));
#21332=CARTESIAN_POINT('Ctrl Pts',(82.257700184868,-4.08359169347408,-0.09571649437622));
#21333=CARTESIAN_POINT('Ctrl Pts',(82.4206859024783,-2.86883663152734,-3.29923455674864));
#21334=CARTESIAN_POINT('Ctrl Pts',(82.6162687636106,1.16238339903618,-4.2168753806827));
#21335=CARTESIAN_POINT('Ctrl Pts',(82.811851624743,4.15031934985653,-1.37057296918483));
#21336=CARTESIAN_POINT('Ctrl Pts',(83.0074344858754,3.44345504116371,2.69406016453184));
#21337=CARTESIAN_POINT('Ctrl Pts',(83.2030173470079,-0.333719683741995,
4.35943641705783));
#21338=CARTESIAN_POINT('Ctrl Pts',(83.39860020814,-3.81263960805445,2.13930714802621));
#21339=CARTESIAN_POINT('Ctrl Pts',(83.5941830692725,-3.8944646466128,-1.98684861864105));
#21340=CARTESIAN_POINT('Ctrl Pts',(83.7897659304049,-0.50564373165627,-4.3426562533637));
#21341=CARTESIAN_POINT('Ctrl Pts',(83.9853487915373,3.3336643879048,-2.8285491238196));
#21342=CARTESIAN_POINT('Ctrl Pts',(84.1809316526696,4.20232603899528,1.20609443396036));
#21343=CARTESIAN_POINT('Ctrl Pts',(84.3765145138021,1.32618441591987,4.16598292634243));
#21344=CARTESIAN_POINT('Ctrl Pts',(84.5720973749343,-2.73173526363988,3.41346879580696));
#21345=CARTESIAN_POINT('Ctrl Pts',(84.7676802360668,-4.35535562891122,-0.380852351780076));
#21346=CARTESIAN_POINT('Ctrl Pts',(84.963263097199,-2.09782657360965,-3.83579056771449));
#21347=CARTESIAN_POINT('Ctrl Pts',(85.1588459583315,2.02911726294498,-3.87257613345951));
#21348=CARTESIAN_POINT('Ctrl Pts',(85.3544288194639,4.34787387083917,-0.458430425156126));
#21349=CARTESIAN_POINT('Ctrl Pts',(85.5500116805963,2.7921507497253,3.36423229852469));
#21350=CARTESIAN_POINT('Ctrl Pts',(85.7455945417287,-1.25171488096045,4.18895863102669));
#21351=CARTESIAN_POINT('Ctrl Pts',(85.9411774028608,-4.18015184799219,1.28081826434192));
#21352=CARTESIAN_POINT('Ctrl Pts',(86.1367602639934,-3.38356990681389,-2.76868550442667));
#21353=CARTESIAN_POINT('Ctrl Pts',(86.3323431251257,0.428180394291547,-4.35095693918743));
#21354=CARTESIAN_POINT('Ctrl Pts',(86.5279259862581,3.85837041772825,-2.05600160947017));
#21355=CARTESIAN_POINT('Ctrl Pts',(86.7235088473905,3.85028754068497,2.07109884112684));
#21356=CARTESIAN_POINT('Ctrl Pts',(86.9190917085228,0.4111347439794,4.3526007156551));
#21357=CARTESIAN_POINT('Ctrl Pts',(87.1146745696552,-3.39438885318226,2.7554110337347));
#21358=CARTESIAN_POINT('Ctrl Pts',(87.3102574307876,-4.17510263508425,-1.29718185414927));
#21359=CARTESIAN_POINT('Ctrl Pts',(87.50584029192,-1.23529790690718,-4.19382935913003));
#21360=CARTESIAN_POINT('Ctrl Pts',(87.7014231530522,2.80530789506251,-3.35326986418407));
#21361=CARTESIAN_POINT('Ctrl Pts',(87.8970060141848,4.34604268780248,0.475457386481673));
#21362=CARTESIAN_POINT('Ctrl Pts',(88.092588875317,2.01393751246173,3.88049411074219));
#21363=CARTESIAN_POINT('Ctrl Pts',(88.2881717364494,-2.11284414771308,3.82754458225146));
#21364=CARTESIAN_POINT('Ctrl Pts',(88.4837545975819,-4.35679539852597,0.36378874697873));
#21365=CARTESIAN_POINT('Ctrl Pts',(88.6793374587141,-2.71838192148609,-3.42414057059281));
#21366=CARTESIAN_POINT('Ctrl Pts',(88.8749203198466,1.34256965287038,-4.16076063290167));
#21367=CARTESIAN_POINT('Ctrl Pts',(89.0705031809788,4.20685975871864,-1.18961625113958));
#21368=CARTESIAN_POINT('Ctrl Pts',(89.2660860421113,3.322882630607,2.84156747674539));
#21369=CARTESIAN_POINT('Ctrl Pts',(89.4616689032436,-0.523309385250935,
4.34067852736659));
#21370=CARTESIAN_POINT('Ctrl Pts',(89.6572517643761,-3.9008702141681,1.97150514629555));
#21371=CARTESIAN_POINT('Ctrl Pts',(89.8528346255084,-3.80698675149828,-2.15407172965046));
#21372=CARTESIAN_POINT('Ctrl Pts',(90.0484174866407,-0.310961962579554,
-4.3610176492037));
#21373=CARTESIAN_POINT('Ctrl Pts',(90.211403204251,2.81536141761182,-2.95949706107794));
#21374=CARTESIAN_POINT('Ctrl Pts',(90.3418371019651,3.81133709361766,-0.644214494217));
#21375=CARTESIAN_POINT('Ctrl Pts',(90.4070767126353,3.71781142410833,0.603927146986502));
#21376=CARTESIAN_POINT('Ctrl Pts',(90.4397191797832,3.52383717212292,1.18211855844504));
#21377=CARTESIAN_POINT('Ctrl Pts',(82.1679464117515,-1.7596983336205,3.54373875243549));
#21378=CARTESIAN_POINT('Ctrl Pts',(82.2005435552736,-2.34034387801246,3.25541021913475));
#21379=CARTESIAN_POINT('Ctrl Pts',(82.2657378423178,-3.35050435026915,2.38818271450672));
#21380=CARTESIAN_POINT('Ctrl Pts',(82.3961264164059,-4.3470115551126,-0.101890869190768));
#21381=CARTESIAN_POINT('Ctrl Pts',(82.5591121340164,-3.05389640372448,-3.51205796704222));
#21382=CARTESIAN_POINT('Ctrl Pts',(82.7546949951485,1.23736515459081,-4.48889296047683));
#21383=CARTESIAN_POINT('Ctrl Pts',(82.950277856281,4.41804360608959,-1.45898438957369));
#21384=CARTESIAN_POINT('Ctrl Pts',(83.1458607174133,3.66558166855189,2.86784564776733));
#21385=CARTESIAN_POINT('Ctrl Pts',(83.3414435785458,-0.355246907694826,
4.64065016808941));
#21386=CARTESIAN_POINT('Ctrl Pts',(83.5370264396781,-4.05858118924538,2.27730723109914));
#21387=CARTESIAN_POINT('Ctrl Pts',(83.7326093008106,-4.14568450779682,-2.1150140738347));
#21388=CARTESIAN_POINT('Ctrl Pts',(83.9281921619428,-0.538261243843927,
-4.62278756796911));
#21389=CARTESIAN_POINT('Ctrl Pts',(84.1237750230752,3.54870876004771,-3.01101007358229));
#21390=CARTESIAN_POINT('Ctrl Pts',(84.3193578842077,4.47340508578664,1.28389585309453));
#21391=CARTESIAN_POINT('Ctrl Pts',(84.5149407453399,1.41173246811791,4.43471759141661));
#21392=CARTESIAN_POINT('Ctrl Pts',(84.7105236064724,-2.90795105091632,3.63366110331307));
#21393=CARTESIAN_POINT('Ctrl Pts',(84.9061064676047,-4.63630614092931,-0.405419958274843));
#21394=CARTESIAN_POINT('Ctrl Pts',(85.101689328737,-2.23315087320723,-4.08322554566206));
#21395=CARTESIAN_POINT('Ctrl Pts',(85.2972721898696,2.16000933756338,-4.12238403440385));
#21396=CARTESIAN_POINT('Ctrl Pts',(85.4928550510018,4.62834175779969,-0.488002353064227));
#21397=CARTESIAN_POINT('Ctrl Pts',(85.6884379121341,2.97226375302626,3.58124851197556));
#21398=CARTESIAN_POINT('Ctrl Pts',(85.8840207732666,-1.33245913393765,4.45917538770145));
#21399=CARTESIAN_POINT('Ctrl Pts',(86.0796036343989,-4.44980050634992,1.36343988650758));
#21400=CARTESIAN_POINT('Ctrl Pts',(86.2751864955313,-3.60183352952659,-2.94728483737715));
#21401=CARTESIAN_POINT('Ctrl Pts',(86.4707693566637,0.455800986330859,-4.63162370534514));
#21402=CARTESIAN_POINT('Ctrl Pts',(86.666352217796,4.10726195191672,-2.18862791007724));
#21403=CARTESIAN_POINT('Ctrl Pts',(86.8619350789284,4.09865767349148,2.20469901742291));
#21404=CARTESIAN_POINT('Ctrl Pts',(87.0575179400608,0.437655773872509,4.63337351674533));
#21405=CARTESIAN_POINT('Ctrl Pts',(87.2531008011932,-3.61335037264109,2.93315407166466));
#21406=CARTESIAN_POINT('Ctrl Pts',(87.4486836623255,-4.44442558434435,-1.38085904084892));
#21407=CARTESIAN_POINT('Ctrl Pts',(87.6442665234579,-1.3149831516979,-4.46436031140006));
#21408=CARTESIAN_POINT('Ctrl Pts',(87.8398493845903,2.98626962508849,-3.56957892492381));
#21409=CARTESIAN_POINT('Ctrl Pts',(88.0354322457226,4.62639245081271,0.506127670967299));
#21410=CARTESIAN_POINT('Ctrl Pts',(88.2310151068551,2.14385038835701,4.13081277589528));
#21411=CARTESIAN_POINT('Ctrl Pts',(88.4265979679873,-2.24913718453744,4.07444763719772));
#21412=CARTESIAN_POINT('Ctrl Pts',(88.6221808291198,-4.63783878562587,0.38725563313876));
#21413=CARTESIAN_POINT('Ctrl Pts',(88.817763690252,-2.89373632598811,-3.64502128126175));
#21414=CARTESIAN_POINT('Ctrl Pts',(89.0133465513846,1.42917466599261,-4.42915842398874));
#21415=CARTESIAN_POINT('Ctrl Pts',(89.2089294125167,4.47823126173771,-1.26635471369913));
#21416=CARTESIAN_POINT('Ctrl Pts',(89.4045122736493,3.53723150495561,3.02486820016417));
#21417=CARTESIAN_POINT('Ctrl Pts',(89.6000951347816,-0.557066454077677,
4.6206822649889));
#21418=CARTESIAN_POINT('Ctrl Pts',(89.795677995914,-4.15250327869021,2.09868084157544));
#21419=CARTESIAN_POINT('Ctrl Pts',(89.9912608570463,-4.05256368440808,-2.29302423018833));
#21420=CARTESIAN_POINT('Ctrl Pts',(90.1868437181788,-0.331021156374193,
-4.64233340062719));
#21421=CARTESIAN_POINT('Ctrl Pts',(90.349829435789,2.99697166926231,-3.150405056996));
#21422=CARTESIAN_POINT('Ctrl Pts',(90.4802633335032,4.05719465363349,-0.685770777428021));
#21423=CARTESIAN_POINT('Ctrl Pts',(90.5455029441732,3.95763593264129,0.642884618114954));
#21424=CARTESIAN_POINT('Ctrl Pts',(90.5781454113212,3.75114900200069,1.25837336805383));
#21425=CARTESIAN_POINT('Ctrl Pts',(82.3063726432896,-1.86633239375375,3.75848195245107));
#21426=CARTESIAN_POINT('Ctrl Pts',(82.3389697868116,-2.48216385081827,3.45268130954456));
#21427=CARTESIAN_POINT('Ctrl Pts',(82.4041640738558,-3.55353794729953,2.53290162133432));
#21428=CARTESIAN_POINT('Ctrl Pts',(82.5345526479439,-4.6104314167511,-0.108065244005317));
#21429=CARTESIAN_POINT('Ctrl Pts',(82.6975383655543,-3.23895617592162,-3.72488137733581));
#21430=CARTESIAN_POINT('Ctrl Pts',(82.8931212266866,1.31234691014545,-4.76091054027098));
#21431=CARTESIAN_POINT('Ctrl Pts',(83.088704087819,4.68576786232264,-1.54739580996254));
#21432=CARTESIAN_POINT('Ctrl Pts',(83.2842869489514,3.88770829594007,3.0416311310028));
#21433=CARTESIAN_POINT('Ctrl Pts',(83.4798698100836,-0.376774131647662,
4.921863919121));
#21434=CARTESIAN_POINT('Ctrl Pts',(83.6754526712162,-4.30452277043632,2.41530731417207));
#21435=CARTESIAN_POINT('Ctrl Pts',(83.8710355323485,-4.39690436898086,-2.24317952902834));
#21436=CARTESIAN_POINT('Ctrl Pts',(84.0666183934809,-0.570878756031578,
-4.90291888257454));
#21437=CARTESIAN_POINT('Ctrl Pts',(84.2622012546133,3.7637531321906,-3.19347102334498));
#21438=CARTESIAN_POINT('Ctrl Pts',(84.4577841157455,4.744484132578,1.3616972722287));
#21439=CARTESIAN_POINT('Ctrl Pts',(84.653366976878,1.49728052031594,4.70345225649081));
#21440=CARTESIAN_POINT('Ctrl Pts',(84.8489498380103,-3.08416683819274,3.85385341081919));
#21441=CARTESIAN_POINT('Ctrl Pts',(85.0445326991427,-4.91725665294739,-0.429987564769618));
#21442=CARTESIAN_POINT('Ctrl Pts',(85.2401155602752,-2.3684751728048,-4.33066052360962));
#21443=CARTESIAN_POINT('Ctrl Pts',(85.4356984214075,2.29090141218177,-4.37219193534821));
#21444=CARTESIAN_POINT('Ctrl Pts',(85.6312812825399,4.90880964476019,-0.517574280972326));
#21445=CARTESIAN_POINT('Ctrl Pts',(85.8268641436722,3.15237675632724,3.79826472542643));
#21446=CARTESIAN_POINT('Ctrl Pts',(86.0224470048046,-1.41320338691484,4.72939214437619));
#21447=CARTESIAN_POINT('Ctrl Pts',(86.2180298659369,-4.71944916470767,1.44606150867324));
#21448=CARTESIAN_POINT('Ctrl Pts',(86.4136127270693,-3.8200971522393,-3.12588417032763));
#21449=CARTESIAN_POINT('Ctrl Pts',(86.6091955882017,0.483421578370174,-4.91229047150286));
#21450=CARTESIAN_POINT('Ctrl Pts',(86.804778449334,4.3561534861052,-2.32125421068431));
#21451=CARTESIAN_POINT('Ctrl Pts',(87.0003613104665,4.347027806298,2.33829919371898));
#21452=CARTESIAN_POINT('Ctrl Pts',(87.1959441715988,0.46417680376561,4.91414631783558));
#21453=CARTESIAN_POINT('Ctrl Pts',(87.3915270327312,-3.83231189209993,3.11089710959462));
#21454=CARTESIAN_POINT('Ctrl Pts',(87.5871098938635,-4.71374853360445,-1.46453622754857));
#21455=CARTESIAN_POINT('Ctrl Pts',(87.782692754996,-1.39466839648862,-4.73489126367011));
#21456=CARTESIAN_POINT('Ctrl Pts',(87.9782756161282,3.16723135511446,-3.78588798566355));
#21457=CARTESIAN_POINT('Ctrl Pts',(88.1738584772607,4.90674221382295,0.536797955452923));
#21458=CARTESIAN_POINT('Ctrl Pts',(88.369441338393,2.27376326425229,4.3811314410484));
#21459=CARTESIAN_POINT('Ctrl Pts',(88.5650241995254,-2.38543022136179,4.32135069214399));
#21460=CARTESIAN_POINT('Ctrl Pts',(88.7606070606577,-4.91888217272578,0.410722519298791));
#21461=CARTESIAN_POINT('Ctrl Pts',(88.9561899217902,-3.06909073049012,-3.86590199193068));
#21462=CARTESIAN_POINT('Ctrl Pts',(89.1517727829225,1.51577967911484,-4.6975562150758));
#21463=CARTESIAN_POINT('Ctrl Pts',(89.3473556440549,4.7496027647568,-1.34309317625867));
#21464=CARTESIAN_POINT('Ctrl Pts',(89.5429385051872,3.75158037930423,3.20816892358296));
#21465=CARTESIAN_POINT('Ctrl Pts',(89.7385213663196,-0.590823522904417,
4.90068600261121));
#21466=CARTESIAN_POINT('Ctrl Pts',(89.934104227452,-4.40413634321233,2.22585653685535));
#21467=CARTESIAN_POINT('Ctrl Pts',(90.1296870885844,-4.2981406173179,-2.43197673072621));
#21468=CARTESIAN_POINT('Ctrl Pts',(90.3252699497168,-0.351080350168827,
-4.92364915205066));
#21469=CARTESIAN_POINT('Ctrl Pts',(90.4882556673271,3.17858192091281,-3.34131305291405));
#21470=CARTESIAN_POINT('Ctrl Pts',(90.6186895650412,4.30305221364934,-0.727327060639044));
#21471=CARTESIAN_POINT('Ctrl Pts',(90.6839291757112,4.19746044117425,0.681842089243407));
#21472=CARTESIAN_POINT('Ctrl Pts',(90.7165716428592,3.97846083187846,1.33462817766261));
#21473=CARTESIAN_POINT('Ctrl Pts',(82.4447988748275,-1.972966453887,3.97322515246666));
#21474=CARTESIAN_POINT('Ctrl Pts',(82.4773960183496,-2.62398382362407,3.64995239995436));
#21475=CARTESIAN_POINT('Ctrl Pts',(82.5425903053937,-3.7565715443299,2.67762052816192));
#21476=CARTESIAN_POINT('Ctrl Pts',(82.6729788794819,-4.87385127838962,-0.114239618819863));
#21477=CARTESIAN_POINT('Ctrl Pts',(82.8359645970922,-3.42401594811876,-3.93770478762939));
#21478=CARTESIAN_POINT('Ctrl Pts',(83.0315474582246,1.38732866570007,-5.03292812006512));
#21479=CARTESIAN_POINT('Ctrl Pts',(83.2271303193571,4.95349211855569,-1.6358072303514));
#21480=CARTESIAN_POINT('Ctrl Pts',(83.4227131804892,4.10983492332825,3.21541661423828));
#21481=CARTESIAN_POINT('Ctrl Pts',(83.6182960416218,-0.398301355600491,
5.20307767015258));
#21482=CARTESIAN_POINT('Ctrl Pts',(83.813878902754,-4.55046435162727,2.55330739724501));
#21483=CARTESIAN_POINT('Ctrl Pts',(84.0094617638865,-4.6481242301649,-2.37134498422198));
#21484=CARTESIAN_POINT('Ctrl Pts',(84.2050446250188,-0.603496268219234,
-5.18305019717995));
#21485=CARTESIAN_POINT('Ctrl Pts',(84.4006274861513,3.9787975043335,-3.37593197310767));
#21486=CARTESIAN_POINT('Ctrl Pts',(84.5962103472836,5.01556317936936,1.43949869136288));
#21487=CARTESIAN_POINT('Ctrl Pts',(84.7917932084159,1.58282857251398,4.97218692156499));
#21488=CARTESIAN_POINT('Ctrl Pts',(84.9873760695484,-3.26038262546918,4.0740457183253));
#21489=CARTESIAN_POINT('Ctrl Pts',(85.1829589306806,-5.19820716496546,-0.454555171264389));
#21490=CARTESIAN_POINT('Ctrl Pts',(85.3785417918131,-2.50379947240239,-4.5780955015572));
#21491=CARTESIAN_POINT('Ctrl Pts',(85.5741246529455,2.42179348680017,-4.62199983629255));
#21492=CARTESIAN_POINT('Ctrl Pts',(85.7697075140778,5.1892775317207,-0.547146208880429));
#21493=CARTESIAN_POINT('Ctrl Pts',(85.9652903752102,3.33248975962821,4.0152809388773));
#21494=CARTESIAN_POINT('Ctrl Pts',(86.1608732363425,-1.49394763989204,4.99960890105093));
#21495=CARTESIAN_POINT('Ctrl Pts',(86.3564560974749,-4.9890978230654,1.52868313083891));
#21496=CARTESIAN_POINT('Ctrl Pts',(86.5520389586073,-4.038360774952,-3.30448350327812));
#21497=CARTESIAN_POINT('Ctrl Pts',(86.7476218197397,0.511042170409484,-5.19295723766057));
#21498=CARTESIAN_POINT('Ctrl Pts',(86.9432046808719,4.60504502029368,-2.45388051129137));
#21499=CARTESIAN_POINT('Ctrl Pts',(87.1387875420045,4.5953979391045,2.47189937001505));
#21500=CARTESIAN_POINT('Ctrl Pts',(87.3343704031367,0.490697833658717,5.19491911892581));
#21501=CARTESIAN_POINT('Ctrl Pts',(87.5299532642692,-4.05127341155876,3.28864014752458));
#21502=CARTESIAN_POINT('Ctrl Pts',(87.7255361254015,-4.98307148286454,-1.54821341424822));
#21503=CARTESIAN_POINT('Ctrl Pts',(87.9211189865339,-1.47435364127935,-5.00542221594014));
#21504=CARTESIAN_POINT('Ctrl Pts',(88.1167018476662,3.34819308514044,-4.00219704640328));
#21505=CARTESIAN_POINT('Ctrl Pts',(88.3122847087986,5.18709197683317,0.567468239938547));
#21506=CARTESIAN_POINT('Ctrl Pts',(88.507867569931,2.40367614014758,4.6314501062015));
#21507=CARTESIAN_POINT('Ctrl Pts',(88.7034504310633,-2.52172325818615,4.56825374709024));
#21508=CARTESIAN_POINT('Ctrl Pts',(88.8990332921958,-5.19992555982569,0.434189405458823));
#21509=CARTESIAN_POINT('Ctrl Pts',(89.0946161533281,-3.24444513499214,-4.08678270259963));
#21510=CARTESIAN_POINT('Ctrl Pts',(89.2901990144604,1.60238469223707,-4.96595400616287));
#21511=CARTESIAN_POINT('Ctrl Pts',(89.4857818755929,5.02097426777587,-1.41983163881822));
#21512=CARTESIAN_POINT('Ctrl Pts',(89.6813647367252,3.96592925365284,3.39146964700175));
#21513=CARTESIAN_POINT('Ctrl Pts',(89.8769475978576,-0.624580591731157,
5.18068974023352));
#21514=CARTESIAN_POINT('Ctrl Pts',(90.0725304589899,-4.65576940773444,2.35303223213525));
#21515=CARTESIAN_POINT('Ctrl Pts',(90.2681133201223,-4.54371755022769,-2.57092923126409));
#21516=CARTESIAN_POINT('Ctrl Pts',(90.4636961812547,-0.371139543963468,
-5.20496490347415));
#21517=CARTESIAN_POINT('Ctrl Pts',(90.626681898865,3.36019217256331,-3.53222104883211));
#21518=CARTESIAN_POINT('Ctrl Pts',(90.7571157965791,4.54890977366517,-0.768883343850067));
#21519=CARTESIAN_POINT('Ctrl Pts',(90.8223554072492,4.43728494970721,0.720799560371859));
#21520=CARTESIAN_POINT('Ctrl Pts',(90.8549978743971,4.20577266175623,1.4108829872714));
#21521=CARTESIAN_POINT('Ctrl Pts',(90.4430005297901,-0.735206482746314,
-4.37679204773777));
#21522=CARTESIAN_POINT('Ctrl Pts',(90.4430005297901,-0.604538703831446,
-4.38932243272125));
#21523=CARTESIAN_POINT('Ctrl Pts',(90.4430005297901,-0.4737103423462,-4.39569211060463));
#21524=CARTESIAN_POINT('Ctrl Pts',(90.4430005297901,-0.343055129970595,
-4.39568396726793));
#21525=CARTESIAN_POINT('Ctrl Pts',(90.4430005297901,-0.334607555765649,
-4.39568344075667));
#21526=CARTESIAN_POINT('Ctrl Pts',(90.4430005297901,-0.326160705233621,
-4.3956562347694));
#21527=CARTESIAN_POINT('Ctrl Pts',(90.4430005297901,-0.317714668695277,
-4.39560228305826));
#21528=CARTESIAN_POINT('Ctrl Pts',(90.4430005297901,-0.185997485435185,
-4.39476089818014));
#21529=CARTESIAN_POINT('Ctrl Pts',(90.4430005297901,-0.0544775308838946,
-4.38741913239467));
#21530=CARTESIAN_POINT('Ctrl Pts',(90.4430005297901,0.0764804063569064,
-4.37382331815595));
#21531=CARTESIAN_POINT('Ctrl Pts',(90.4430005297901,0.212139516582048,-4.35973943671073));
#21532=CARTESIAN_POINT('Ctrl Pts',(90.4430005297901,0.347196453092427,-4.33894421155611));
#21533=CARTESIAN_POINT('Ctrl Pts',(90.4430005297901,0.481228112669947,-4.3116562756427));
#21534=CARTESIAN_POINT('Ctrl Pts',(90.4430005297901,0.615259772247468,-4.2843683397293));
#21535=CARTESIAN_POINT('Ctrl Pts',(90.4430005297901,0.748267008611165,-4.25058714871171));
#21536=CARTESIAN_POINT('Ctrl Pts',(90.4430005297901,0.8797960890982,-4.2104833822017));
#21537=CARTESIAN_POINT('Ctrl Pts',(90.4430005297901,0.896953403142723,-4.20525204542178));
#21538=CARTESIAN_POINT('Ctrl Pts',(90.4430005297901,0.91408551176748,-4.19991306416615));
#21539=CARTESIAN_POINT('Ctrl Pts',(90.4430005297901,0.931191357547314,-4.19446676463672));
#21540=CARTESIAN_POINT('Ctrl Pts',(90.4430005297901,0.947772132258863,-4.18918764154211));
#21541=CARTESIAN_POINT('Ctrl Pts',(90.4430005297901,0.964318662466662,-4.18381073214009));
#21542=CARTESIAN_POINT('Ctrl Pts',(90.4430005297901,0.980829620677612,-4.17833682356824));
#21543=CARTESIAN_POINT('Ctrl Pts',(90.4430005297901,1.10554259859417,-4.13699049889609));
#21544=CARTESIAN_POINT('Ctrl Pts',(90.4430005297901,1.22823748709574,-4.09011104027403));
#21545=CARTESIAN_POINT('Ctrl Pts',(90.4430005297901,1.3485575220433,-4.03793699452255));
#21546=CARTESIAN_POINT('Ctrl Pts',(90.4430005297901,1.4690034609849,-3.98570835336851));
#21547=CARTESIAN_POINT('Ctrl Pts',(90.4430005297901,1.58707030875767,-3.92817353589151));
#21548=CARTESIAN_POINT('Ctrl Pts',(90.4430005297901,1.70237501425449,-3.86552606398859));
#21549=CARTESIAN_POINT('Ctrl Pts',(90.4430005297901,1.81579371193992,-3.80390329980132));
#21550=CARTESIAN_POINT('Ctrl Pts',(90.4430005297901,1.92654047357856,-3.73733320225429));
#21551=CARTESIAN_POINT('Ctrl Pts',(90.4430005297901,2.03421675054925,-3.66596377326627));
#21552=CARTESIAN_POINT('Ctrl Pts',(90.4430005297901,2.12284103122993,-3.60722228921239));
#21553=CARTESIAN_POINT('Ctrl Pts',(90.4430005297901,2.20938482207715,-3.54522882338617));
#21554=CARTESIAN_POINT('Ctrl Pts',(90.4430005297901,2.29360397058158,-3.48005089866155));
#21555=CARTESIAN_POINT('Ctrl Pts',(90.4430005297901,2.31916577926078,-3.46026839466449));
#21556=CARTESIAN_POINT('Ctrl Pts',(90.4430005297901,2.34451328416945,-3.44019244944633));
#21557=CARTESIAN_POINT('Ctrl Pts',(90.4430005297901,2.36963923936791,-3.41982474290588));
#21558=CARTESIAN_POINT('Ctrl Pts',(90.4430005297901,2.38341896005213,-3.40865456828412));
#21559=CARTESIAN_POINT('Ctrl Pts',(90.4430005297901,2.39712536031612,-3.39740203463942));
#21560=CARTESIAN_POINT('Ctrl Pts',(90.4430005297901,2.4107546065151,-3.38607005694199));
#21561=CARTESIAN_POINT('Ctrl Pts',(90.4430005297901,2.46077454371223,-3.34448119689286));
#21562=CARTESIAN_POINT('Ctrl Pts',(90.4430005297901,2.50976810825464,-3.30181224193952));
#21563=CARTESIAN_POINT('Ctrl Pts',(90.4430005297901,2.55768970288188,-3.25808790138363));
#21564=CARTESIAN_POINT('Ctrl Pts',(90.4430005297901,2.65095689235614,-3.17298959889633));
#21565=CARTESIAN_POINT('Ctrl Pts',(90.4430005297901,2.74016608735159,-3.08389558277388));
#21566=CARTESIAN_POINT('Ctrl Pts',(90.4430005297901,2.82495239396308,-2.99096257965398));
#21567=CARTESIAN_POINT('Ctrl Pts',(90.4430005297901,2.90759162314816,-2.90038295600232));
#21568=CARTESIAN_POINT('Ctrl Pts',(90.4430005297901,2.98602952066637,-2.80615579142114));
#21569=CARTESIAN_POINT('Ctrl Pts',(90.4430005297901,3.05988679011808,-2.70840035946947));
#21570=CARTESIAN_POINT('Ctrl Pts',(90.4430005297901,3.11277433976829,-2.63839986663643));
#21571=CARTESIAN_POINT('Ctrl Pts',(90.4430005297901,3.16331226028424,-2.56658964974082));
#21572=CARTESIAN_POINT('Ctrl Pts',(90.4430005297901,3.2113460253676,-2.49300717327591));
#21573=CARTESIAN_POINT('Ctrl Pts',(90.4430005297901,3.25596252339907,-2.42465957631677));
#21574=CARTESIAN_POINT('Ctrl Pts',(90.4430005297901,3.29841825709039,-2.354782644304));
#21575=CARTESIAN_POINT('Ctrl Pts',(90.4430005297901,3.33867108373867,-2.28349579149761));
#21576=CARTESIAN_POINT('Ctrl Pts',(90.4430005297901,3.35066966420012,-2.26224657472299));
#21577=CARTESIAN_POINT('Ctrl Pts',(90.4430005297901,3.36247245082681,-2.24087208124526));
#21578=CARTESIAN_POINT('Ctrl Pts',(90.4430005297901,3.37407817045466,-2.21937547389451));
#21579=CARTESIAN_POINT('Ctrl Pts',(90.4430005297901,3.38225827070718,-2.20422394440242));
#21580=CARTESIAN_POINT('Ctrl Pts',(90.4430005297901,3.39034041097382,-2.18901172139937));
#21581=CARTESIAN_POINT('Ctrl Pts',(90.4430005297901,3.39831759446147,-2.17375281910387));
#21582=CARTESIAN_POINT('Ctrl Pts',(90.4430005297901,3.4551234429507,-2.06509355443337));
#21583=CARTESIAN_POINT('Ctrl Pts',(90.4430005297901,3.50669909621418,-1.95390743199697));
#21584=CARTESIAN_POINT('Ctrl Pts',(90.4430005297901,3.55299874508288,-1.84063291121359));
#21585=CARTESIAN_POINT('Ctrl Pts',(90.4430005297901,3.59985305587428,-1.72600138092743));
#21586=CARTESIAN_POINT('Ctrl Pts',(90.4430005297901,3.64130438566013,-1.6092302210154));
#21587=CARTESIAN_POINT('Ctrl Pts',(90.4430005297901,3.67725474073973,-1.49075882570099));
#21588=CARTESIAN_POINT('Ctrl Pts',(90.4430005297901,3.71297351100698,-1.37305059881123));
#21589=CARTESIAN_POINT('Ctrl Pts',(90.4430005297901,3.74326199392705,-1.25366307552021));
#21590=CARTESIAN_POINT('Ctrl Pts',(90.4430005297901,3.76797297501044,-1.1330259641585));
#21591=CARTESIAN_POINT('Ctrl Pts',(90.4430005297901,3.78309861206878,-1.05918376598491));
#21592=CARTESIAN_POINT('Ctrl Pts',(90.4430005297901,3.79613353366921,-0.98487341865883));
#21593=CARTESIAN_POINT('Ctrl Pts',(90.4430005297901,3.80703431601147,-0.910195398393028));
#21594=CARTESIAN_POINT('Ctrl Pts',(90.4430005297901,3.81275326778124,-0.87101655941134));
#21595=CARTESIAN_POINT('Ctrl Pts',(90.4430005297901,3.81788468776157,-0.831736555533261));
#21596=CARTESIAN_POINT('Ctrl Pts',(90.4430005297901,3.82242148213659,-0.79237018659198));
#21597=CARTESIAN_POINT('Ctrl Pts',(90.4430005297901,3.82477895958205,-0.771914040860599));
#21598=CARTESIAN_POINT('Ctrl Pts',(90.4430005297901,3.82697612959026,-0.751431871386733));
#21599=CARTESIAN_POINT('Ctrl Pts',(90.4430005297901,3.82901104070976,-0.730934968196635));
#21600=CARTESIAN_POINT('Ctrl Pts',(90.4430005297901,3.83052437597813,-0.715691704649236));
#21601=CARTESIAN_POINT('Ctrl Pts',(90.4430005297901,3.83194777392774,-0.70044244785746));
#21602=CARTESIAN_POINT('Ctrl Pts',(90.4430005297901,3.83328081539605,-0.685190377817854));
#21603=CARTESIAN_POINT('Ctrl Pts',(90.4430005297901,3.83425091868926,-0.674090885622495));
#21604=CARTESIAN_POINT('Ctrl Pts',(90.4430005297901,3.83517321726714,-0.66298940552743));
#21605=CARTESIAN_POINT('Ctrl Pts',(90.4430005297901,3.83604763234583,-0.6518862628284));
#21606=CARTESIAN_POINT('Ctrl Pts',(90.4430005297901,3.84560195174611,-0.530567481532555));
#21607=CARTESIAN_POINT('Ctrl Pts',(90.4430005297901,3.84944379015736,-0.40904962007089));
#21608=CARTESIAN_POINT('Ctrl Pts',(90.4430005297901,3.84760828244277,-0.287700071444294));
#21609=CARTESIAN_POINT('Ctrl Pts',(90.4430005297901,3.84578233258688,-0.166982414381175));
#21610=CARTESIAN_POINT('Ctrl Pts',(90.4430005297901,3.8383377921992,-0.0464305630719454));
#21611=CARTESIAN_POINT('Ctrl Pts',(90.4430005297901,3.82525995553925,0.0735799560127684));
#21612=CARTESIAN_POINT('Ctrl Pts',(90.4430005297901,3.82045107314999,0.117709309112766));
#21613=CARTESIAN_POINT('Ctrl Pts',(90.4430005297901,3.81488003310189,0.16176527531321));
#21614=CARTESIAN_POINT('Ctrl Pts',(90.4430005297901,3.80854450228284,0.205728399455385));
#21615=CARTESIAN_POINT('Ctrl Pts',(90.4430005297901,3.8042331526489,0.235645450542403));
#21616=CARTESIAN_POINT('Ctrl Pts',(90.4430005297901,3.79956659035794,0.265525695687981));
#21617=CARTESIAN_POINT('Ctrl Pts',(90.4430005297901,3.79455002103167,0.29532852943585));
#21618=CARTESIAN_POINT('Ctrl Pts',(90.4430005297901,3.77482815798568,0.412493740824486));
#21619=CARTESIAN_POINT('Ctrl Pts',(90.4430005297901,3.74969110993674,0.528545803738649));
#21620=CARTESIAN_POINT('Ctrl Pts',(90.4430005297901,3.71914658870853,0.643128875915091));
#21621=CARTESIAN_POINT('Ctrl Pts',(90.4430005297901,3.68911896823763,0.75577287442469));
#21622=CARTESIAN_POINT('Ctrl Pts',(90.4430005297901,3.65386504700212,0.86699780500097));
#21623=CARTESIAN_POINT('Ctrl Pts',(90.4430005297901,3.61334804287102,0.97644236203363));
#21624=CARTESIAN_POINT('Ctrl Pts',(90.4430005297901,3.58775745478563,1.04556767465913));
#21625=CARTESIAN_POINT('Ctrl Pts',(90.4430005297901,3.56006645271635,1.11398226507298));
#21626=CARTESIAN_POINT('Ctrl Pts',(90.4430005297901,3.5302572329849,1.18158852036477));
#21627=CARTESIAN_POINT('Ctrl Pts',(82.4430005297901,-2.16672251220859,-3.03255290461516));
#21628=CARTESIAN_POINT('Ctrl Pts',(82.4430005297901,-2.2696406448299,-2.9735626011528));
#21629=CARTESIAN_POINT('Ctrl Pts',(82.4430005297901,-2.36930641006409,-2.90958285743481));
#21630=CARTESIAN_POINT('Ctrl Pts',(82.4430005297901,-2.4652895168029,-2.84070661811296));
#21631=CARTESIAN_POINT('Ctrl Pts',(82.4430005297901,-2.55923374195207,-2.77329345392055));
#21632=CARTESIAN_POINT('Ctrl Pts',(82.4430005297901,-2.64965127392472,-2.70118974547307));
#21633=CARTESIAN_POINT('Ctrl Pts',(82.4430005297901,-2.73645513109191,-2.62479035097945));
#21634=CARTESIAN_POINT('Ctrl Pts',(82.4430005297901,-2.79259033985632,-2.57538360686307));
#21635=CARTESIAN_POINT('Ctrl Pts',(82.4430005297901,-2.84721383859095,-2.52417932868561));
#21636=CARTESIAN_POINT('Ctrl Pts',(82.4430005297901,-2.90029628102234,-2.47127435007986));
#21637=CARTESIAN_POINT('Ctrl Pts',(82.4430005297901,-2.91981754671394,-2.45181834737037));
#21638=CARTESIAN_POINT('Ctrl Pts',(82.4430005297901,-2.93913346768778,-2.43212884764077));
#21639=CARTESIAN_POINT('Ctrl Pts',(82.4430005297901,-2.95822228666816,-2.41223190685226));
#21640=CARTESIAN_POINT('Ctrl Pts',(82.4430005297901,-3.03989891485165,-2.32709751292032));
#21641=CARTESIAN_POINT('Ctrl Pts',(82.4430005297901,-3.11748745097799,-2.23810423358288));
#21642=CARTESIAN_POINT('Ctrl Pts',(82.4430005297901,-3.19090385621255,-2.14566782445364));
#21643=CARTESIAN_POINT('Ctrl Pts',(82.4430005297901,-3.2660819932855,-2.0510132712397));
#21644=CARTESIAN_POINT('Ctrl Pts',(82.4430005297901,-3.33688589309288,-1.95274786922678));
#21645=CARTESIAN_POINT('Ctrl Pts',(82.4430005297901,-3.40319502447745,-1.85127235969848));
#21646=CARTESIAN_POINT('Ctrl Pts',(82.4430005297901,-3.44327359760755,-1.78993852008059));
#21647=CARTESIAN_POINT('Ctrl Pts',(82.4430005297901,-3.48170950646411,-1.72743110356979));
#21648=CARTESIAN_POINT('Ctrl Pts',(82.4430005297901,-3.51846970607509,-1.66383203062367));
#21649=CARTESIAN_POINT('Ctrl Pts',(82.4430005297901,-3.52766288301639,-1.64792685227634));
#21650=CARTESIAN_POINT('Ctrl Pts',(82.4430005297901,-3.53674997798665,-1.63195544603767));
#21651=CARTESIAN_POINT('Ctrl Pts',(82.4430005297901,-3.54572521930434,-1.61592885171508));
#21652=CARTESIAN_POINT('Ctrl Pts',(82.4430005297901,-3.60610285231906,-1.50811583630591));
#21653=CARTESIAN_POINT('Ctrl Pts',(82.4430005297901,-3.66149200213407,-1.39768708900077));
#21654=CARTESIAN_POINT('Ctrl Pts',(82.4430005297901,-3.71180063322066,-1.28507982535995));
#21655=CARTESIAN_POINT('Ctrl Pts',(82.4430005297901,-3.76266962345599,-1.17121829363366));
#21656=CARTESIAN_POINT('Ctrl Pts',(82.4430005297901,-3.8083447828333,-1.05512876825121));
#21657=CARTESIAN_POINT('Ctrl Pts',(82.4430005297901,-3.84869498052848,-0.937223070177858));
#21658=CARTESIAN_POINT('Ctrl Pts',(82.4430005297901,-3.88901078279322,-0.819417877615471));
#21659=CARTESIAN_POINT('Ctrl Pts',(82.4430005297901,-3.92401114105584,-0.699798835821216));
#21660=CARTESIAN_POINT('Ctrl Pts',(82.4430005297901,-3.95352257290869,-0.578747854386884));
#21661=CARTESIAN_POINT('Ctrl Pts',(82.4430005297901,-3.97523656822446,-0.489680659784435));
#21662=CARTESIAN_POINT('Ctrl Pts',(82.4430005297901,-3.99397814296339,-0.399837595278188));
#21663=CARTESIAN_POINT('Ctrl Pts',(82.4430005297901,-4.00966125689264,-0.309364507448106));
#21664=CARTESIAN_POINT('Ctrl Pts',(82.4430005297901,-4.01435795168095,-0.282270112673519));
#21665=CARTESIAN_POINT('Ctrl Pts',(82.4430005297901,-4.01878024374387,-0.255119189321616));
#21666=CARTESIAN_POINT('Ctrl Pts',(82.4430005297901,-4.02292554754272,-0.227915601567328));
#21667=CARTESIAN_POINT('Ctrl Pts',(82.4430005297901,-4.02569591908626,-0.20973501721123));
#21668=CARTESIAN_POINT('Ctrl Pts',(82.4430005297901,-4.02834281759651,-0.191528743140453));
#21669=CARTESIAN_POINT('Ctrl Pts',(82.4430005297901,-4.03086308406066,-0.173316124913731));
#21670=CARTESIAN_POINT('Ctrl Pts',(82.4430005297901,-4.04843750869992,-0.046315154555558));
#21671=CARTESIAN_POINT('Ctrl Pts',(82.4430005297901,-4.05988667809022,0.0811706755403835));
#21672=CARTESIAN_POINT('Ctrl Pts',(82.4430005297901,-4.06508069808529,0.20871668428979));
#21673=CARTESIAN_POINT('Ctrl Pts',(82.4430005297901,-4.0692831193649,0.311912679262398));
#21674=CARTESIAN_POINT('Ctrl Pts',(82.4430005297901,-4.06939010281968,0.415148898919295));
#21675=CARTESIAN_POINT('Ctrl Pts',(82.4430005297901,-4.06531043519685,0.518211439887901));
#21676=CARTESIAN_POINT('Ctrl Pts',(82.4430005297901,-4.06037373247765,0.642924816879996));
#21677=CARTESIAN_POINT('Ctrl Pts',(82.4430005297901,-4.04930850365814,0.767384162347737));
#21678=CARTESIAN_POINT('Ctrl Pts',(82.4430005297901,-4.03236186892168,0.891221661938483));
#21679=CARTESIAN_POINT('Ctrl Pts',(82.4430005297901,-4.01541523418522,1.01505916152923));
#21680=CARTESIAN_POINT('Ctrl Pts',(82.4430005297901,-3.9925869512816,1.13827557220802));
#21681=CARTESIAN_POINT('Ctrl Pts',(82.4430005297901,-3.96407180720897,1.26050316969768));
#21682=CARTESIAN_POINT('Ctrl Pts',(82.4430005297901,-3.95547258916304,1.29736294355562));
#21683=CARTESIAN_POINT('Ctrl Pts',(82.4430005297901,-3.9463558470242,1.33413274985256));
#21684=CARTESIAN_POINT('Ctrl Pts',(82.4430005297901,-3.93672603994556,1.37080234332704));
#21685=CARTESIAN_POINT('Ctrl Pts',(82.4430005297901,-3.93229805917785,1.38766376675315));
#21686=CARTESIAN_POINT('Ctrl Pts',(82.4430005297901,-3.92776385858573,1.40449532876003));
#21687=CARTESIAN_POINT('Ctrl Pts',(82.4430005297901,-3.92312493683007,1.42129347051884));
#21688=CARTESIAN_POINT('Ctrl Pts',(82.4430005297901,-3.88922045173003,1.54406604073413));
#21689=CARTESIAN_POINT('Ctrl Pts',(82.4430005297901,-3.84971460163609,1.66509780758731));
#21690=CARTESIAN_POINT('Ctrl Pts',(82.4430005297901,-3.80489648217205,1.78401656479781));
#21691=CARTESIAN_POINT('Ctrl Pts',(82.4430005297901,-3.75909623686104,1.90554125877099));
#21692=CARTESIAN_POINT('Ctrl Pts',(82.4430005297901,-3.70774825327871,2.02486010777613));
#21693=CARTESIAN_POINT('Ctrl Pts',(82.4430005297901,-3.65110614357196,2.14157776463153));
#21694=CARTESIAN_POINT('Ctrl Pts',(82.4430005297901,-3.59646760585506,2.2541668283041));
#21695=CARTESIAN_POINT('Ctrl Pts',(82.4430005297901,-3.53690231335205,2.36433614459377));
#21696=CARTESIAN_POINT('Ctrl Pts',(82.4430005297901,-3.47259286055702,2.47172179522677));
#21697=CARTESIAN_POINT('Ctrl Pts',(82.4430005297901,-3.40566020000047,2.58348774859871));
#21698=CARTESIAN_POINT('Ctrl Pts',(82.4430005297901,-3.33358842352915,2.69223917331593));
#21699=CARTESIAN_POINT('Ctrl Pts',(82.4430005297901,-3.25661397611833,2.79770775568242));
#21700=CARTESIAN_POINT('Ctrl Pts',(82.4430005297901,-3.2459176943,2.81236355014302));
#21701=CARTESIAN_POINT('Ctrl Pts',(82.4430005297901,-3.23512667474306,2.82695590898395));
#21702=CARTESIAN_POINT('Ctrl Pts',(82.4430005297901,-3.22424148623506,2.84148406610821));
#21703=CARTESIAN_POINT('Ctrl Pts',(82.4430005297901,-3.20381603969898,2.86874533920342));
#21704=CARTESIAN_POINT('Ctrl Pts',(82.4430005297901,-3.18308002897164,2.89575244319934));
#21705=CARTESIAN_POINT('Ctrl Pts',(82.4430005297901,-3.16204383972264,2.92249587205561));
#21706=CARTESIAN_POINT('Ctrl Pts',(82.4430005297901,-3.07995910811394,3.02685066531118));
#21707=CARTESIAN_POINT('Ctrl Pts',(82.4430005297901,-2.99328647074254,3.12722044563493));
#21708=CARTESIAN_POINT('Ctrl Pts',(82.4430005297901,-2.90235593084009,3.22337065901414));
#21709=CARTESIAN_POINT('Ctrl Pts',(82.4430005297901,-2.81091979211652,3.32005549403519));
#21710=CARTESIAN_POINT('Ctrl Pts',(82.4430005297901,-2.71517785948218,3.41247434460212));
#21711=CARTESIAN_POINT('Ctrl Pts',(82.4430005297901,-2.6154171072342,3.50036721001472));
#21712=CARTESIAN_POINT('Ctrl Pts',(82.4430005297901,-2.51634883740782,3.58764997312848));
#21713=CARTESIAN_POINT('Ctrl Pts',(82.4430005297901,-2.41331685430689,3.6704699525819));
#21714=CARTESIAN_POINT('Ctrl Pts',(82.4430005297901,-2.30656133318296,3.74854230234771));
#21715=CARTESIAN_POINT('Ctrl Pts',(82.4430005297901,-2.20467684379054,3.82305237365655));
#21716=CARTESIAN_POINT('Ctrl Pts',(82.4430005297901,-2.09940025075541,3.8932384548752));
#21717=CARTESIAN_POINT('Ctrl Pts',(82.4430005297901,-1.99091130097234,3.9588194824242));
#21718=CARTESIAN_POINT('Ctrl Pts',(82.4430005297901,-1.98447919887494,3.96270765597266));
#21719=CARTESIAN_POINT('Ctrl Pts',(82.4430005297901,-1.97803579776512,3.96657963149843));
#21720=CARTESIAN_POINT('Ctrl Pts',(82.4430005297901,-1.97158113240045,3.97043534620103));
#21721=CARTESIAN_POINT('Ctrl Pts',(82.0310032950812,2.5732449024852,-3.61351950356445));
#21722=CARTESIAN_POINT('Ctrl Pts',(82.0636457680076,3.16616325925722,-3.19130979057643));
#21723=CARTESIAN_POINT('Ctrl Pts',(82.1288853844562,4.13207912470726,-2.05174262577274));
#21724=CARTESIAN_POINT('Ctrl Pts',(82.2593192879487,4.79464520668388,0.882555540610264));
#21725=CARTESIAN_POINT('Ctrl Pts',(82.4223050055592,2.75914274104666,4.42905501007769));
#21726=CARTESIAN_POINT('Ctrl Pts',(82.6178878666914,-2.16479008544544,4.75065483431134));
#21727=CARTESIAN_POINT('Ctrl Pts',(82.8134707278238,-5.14967299145611,0.832949191282387));
#21728=CARTESIAN_POINT('Ctrl Pts',(83.0090535889562,-3.55042897662582,-3.82414592282758));
#21729=CARTESIAN_POINT('Ctrl Pts',(83.2046364500884,1.21504830394734,-5.0748705164238));
#21730=CARTESIAN_POINT('Ctrl Pts',(83.400219311221,4.89660859864141,-1.80258629906098));
#21731=CARTESIAN_POINT('Ctrl Pts',(83.5958021723532,4.21527029670854,3.07568249282053));
#21732=CARTESIAN_POINT('Ctrl Pts',(83.7913850334858,-0.222660655853561,
5.21331275103613));
#21733=CARTESIAN_POINT('Ctrl Pts',(83.9869678946179,-4.46203744762071,2.7051724468734));
#21734=CARTESIAN_POINT('Ctrl Pts',(84.1825507557504,-4.72526831706301,-2.21356276749624));
#21735=CARTESIAN_POINT('Ctrl Pts',(84.3781336168827,-0.777683074796472,
-5.15976630774078));
#21736=CARTESIAN_POINT('Ctrl Pts',(84.5737164780151,3.86289539882142,-3.50798698251897));
#21737=CARTESIAN_POINT('Ctrl Pts',(84.7692993391475,5.06117659898468,1.26982667827935));
#21738=CARTESIAN_POINT('Ctrl Pts',(84.96488220028,1.74933589258655,4.91607408021796));
#21739=CARTESIAN_POINT('Ctrl Pts',(85.1604650614123,-3.12137193940479,4.18150613925552));
#21740=CARTESIAN_POINT('Ctrl Pts',(85.3560479225446,-5.21056228074381,-0.279286952965116));
#21741=CARTESIAN_POINT('Ctrl Pts',(85.5516307836769,-2.65651348040282,-4.49120199383985));
#21742=CARTESIAN_POINT('Ctrl Pts',(85.7472136448093,2.26480862632819,-4.70091489012678));
#21743=CARTESIAN_POINT('Ctrl Pts',(85.9427965059417,5.16791352719978,-0.721546383514633));
#21744=CARTESIAN_POINT('Ctrl Pts',(86.1383793670741,3.46578485734584,3.90080690363208));
#21745=CARTESIAN_POINT('Ctrl Pts',(86.3339622282066,-1.32477558834876,5.04707131090363));
#21746=CARTESIAN_POINT('Ctrl Pts',(86.5295450893389,-4.93480143762726,1.69578718575462));
#21747=CARTESIAN_POINT('Ctrl Pts',(86.7251279504711,-4.14732466254241,-3.16664760615603));
#21748=CARTESIAN_POINT('Ctrl Pts',(86.9207108116036,0.335917868796414,-5.20721791424714));
#21749=CARTESIAN_POINT('Ctrl Pts',(87.1162936727359,4.51981737154225,-2.60752975275673));
#21750=CARTESIAN_POINT('Ctrl Pts',(87.3118765338683,4.67601458569188,2.3157815033228));
#21751=CARTESIAN_POINT('Ctrl Pts',(87.5074593950007,0.665320577523391,5.17545253638813));
#21752=CARTESIAN_POINT('Ctrl Pts',(87.7030422561331,-3.93825640509612,3.42317175243948));
#21753=CARTESIAN_POINT('Ctrl Pts',(87.8986251172654,-5.03236803225271,-1.37956714940564));
#21754=CARTESIAN_POINT('Ctrl Pts',(88.0942079783978,-1.64204264387256,-4.95294612034352));
#21755=CARTESIAN_POINT('Ctrl Pts',(88.2897908395301,3.21155918647893,-4.11265223251709));
#21756=CARTESIAN_POINT('Ctrl Pts',(88.4853737006626,5.20323685809616,0.39250777042273));
#21757=CARTESIAN_POINT('Ctrl Pts',(88.6809565617948,2.55828132447017,4.54790108430783));
#21758=CARTESIAN_POINT('Ctrl Pts',(88.8765394229273,-2.36656955065493,4.65055642185629));
#21759=CARTESIAN_POINT('Ctrl Pts',(89.0721222840597,-5.1821983422279,0.609026662521216));
#21760=CARTESIAN_POINT('Ctrl Pts',(89.2677051451921,-3.38052451202556,-3.97526189866621));
#21761=CARTESIAN_POINT('Ctrl Pts',(89.4632880063243,1.43495189680254,-5.01702611225074));
#21762=CARTESIAN_POINT('Ctrl Pts',(89.6588708674568,4.96896142408185,-1.58819351471315));
#21763=CARTESIAN_POINT('Ctrl Pts',(89.8544537285891,4.08065273654629,3.25627251816026));
#21764=CARTESIAN_POINT('Ctrl Pts',(90.0500365897215,-0.455561874102168,
5.19825550801701));
#21765=CARTESIAN_POINT('Ctrl Pts',(90.2130223073318,-3.87588474101625,2.95720212609757));
#21766=CARTESIAN_POINT('Ctrl Pts',(90.3434108814201,-4.6129921626674,0.0418147320781305));
#21767=CARTESIAN_POINT('Ctrl Pts',(90.4086051684642,-4.26823548650425,-1.41053445637093));
#21768=CARTESIAN_POINT('Ctrl Pts',(90.4412023119862,-3.93156634387324,-2.05472598388759));
#21769=CARTESIAN_POINT('Ctrl Pts',(82.1694296294366,2.43416713531397,-3.41821736823327));
#21770=CARTESIAN_POINT('Ctrl Pts',(82.202072102363,2.99503966500787,-3.01882708611391));
#21771=CARTESIAN_POINT('Ctrl Pts',(82.2673117188115,3.9087500751154,-1.94085081639738));
#21772=CARTESIAN_POINT('Ctrl Pts',(82.3977456223042,4.53550603610597,0.834855512574021));
#21773=CARTESIAN_POINT('Ctrl Pts',(82.5607313399144,2.61001763781187,4.18967512016311));
#21774=CARTESIAN_POINT('Ctrl Pts',(82.7563142010469,-2.04778832972938,4.49389323874026));
#21775=CARTESIAN_POINT('Ctrl Pts',(82.9518970621792,-4.8713454134545,0.787930268451231));
#21776=CARTESIAN_POINT('Ctrl Pts',(83.1474799233117,-3.3585367342309,-3.61745993045656));
#21777=CARTESIAN_POINT('Ctrl Pts',(83.3430627844438,1.14937783280214,-4.80058583429903));
#21778=CARTESIAN_POINT('Ctrl Pts',(83.5386456455763,4.63195854922217,-1.70516079658948));
#21779=CARTESIAN_POINT('Ctrl Pts',(83.7342285067087,3.98744496211903,2.90944916881162));
#21780=CARTESIAN_POINT('Ctrl Pts',(83.9298113678411,-0.210626376946379,
4.93154559538018));
#21781=CARTESIAN_POINT('Ctrl Pts',(84.1253942289734,-4.22087493539727,2.55896430968406));
#21782=CARTESIAN_POINT('Ctrl Pts',(84.3209770901058,-4.46987880237384,-2.09392496430875));
#21783=CARTESIAN_POINT('Ctrl Pts',(84.5165599512381,-0.735651154124987,
-4.88089320999837));
#21784=CARTESIAN_POINT('Ctrl Pts',(84.7121428123705,3.6541150894287,-3.31838862896805));
#21785=CARTESIAN_POINT('Ctrl Pts',(84.9077256735029,4.78763204053,1.20119556627793));
#21786=CARTESIAN_POINT('Ctrl Pts',(85.1033085346353,1.65478844794245,4.65037196781321));
#21787=CARTESIAN_POINT('Ctrl Pts',(85.2988913957676,-2.95266920946872,3.95550567707689));
#21788=CARTESIAN_POINT('Ctrl Pts',(85.4944742569001,-4.92894378146587,-0.264192157370293));
#21789=CARTESIAN_POINT('Ctrl Pts',(85.6900571180323,-2.51293524462826,-4.24846320725372));
#21790=CARTESIAN_POINT('Ctrl Pts',(85.8856399791648,2.14240110634607,-4.44684162024508));
#21791=CARTESIAN_POINT('Ctrl Pts',(86.0812228402971,4.88860009162169,-0.682548517500101));
#21792=CARTESIAN_POINT('Ctrl Pts',(86.2768057014295,3.27846742829351,3.6899775675672));
#21793=CARTESIAN_POINT('Ctrl Pts',(86.4723885625619,-1.25317461844009,4.7742891097239));
#21794=CARTESIAN_POINT('Ctrl Pts',(86.6679714236942,-4.6680871560928,1.60413392136281));
#21795=CARTESIAN_POINT('Ctrl Pts',(86.8635542848266,-3.92317162788817,-2.9954978341087));
#21796=CARTESIAN_POINT('Ctrl Pts',(87.0591371459591,0.31776230688313,-4.92578017002461));
#21797=CARTESIAN_POINT('Ctrl Pts',(87.2547200070913,4.27553199184569,-2.46659897096611));
#21798=CARTESIAN_POINT('Ctrl Pts',(87.4503028682238,4.42328711804585,2.19061902056514));
#21799=CARTESIAN_POINT('Ctrl Pts',(87.645885729356,0.62936158260391,4.89573163529303));
#21800=CARTESIAN_POINT('Ctrl Pts',(87.8414685904886,-3.72540301254123,3.23815746036292));
#21801=CARTESIAN_POINT('Ctrl Pts',(88.0370514516208,-4.76038050831605,-1.30500482592964));
#21802=CARTESIAN_POINT('Ctrl Pts',(88.2326343127533,-1.55329414415176,-4.68525116186073));
#21803=CARTESIAN_POINT('Ctrl Pts',(88.4282171738855,3.03798205032592,-3.89037316024618));
#21804=CARTESIAN_POINT('Ctrl Pts',(88.623800035018,4.92201428049067,0.371293658911228));
#21805=CARTESIAN_POINT('Ctrl Pts',(88.8193828961503,2.42001230310359,4.30209784672624));
#21806=CARTESIAN_POINT('Ctrl Pts',(89.0149657572827,-2.23866209472541,4.39920490741982));
#21807=CARTESIAN_POINT('Ctrl Pts',(89.2105486184151,-4.90211284637034,0.576110219826852));
#21808=CARTESIAN_POINT('Ctrl Pts',(89.4061314795474,-3.19781520186777,-3.760408447192));
#21809=CARTESIAN_POINT('Ctrl Pts',(89.6017143406798,1.35739615944824,-4.74586778260333));
#21810=CARTESIAN_POINT('Ctrl Pts',(89.7972972018122,4.70040087652035,-1.50235543235697));
#21811=CARTESIAN_POINT('Ctrl Pts',(89.9928800629445,3.86010316092995,3.08027873276914));
#21812=CARTESIAN_POINT('Ctrl Pts',(90.188462924077,-0.430939838244923,4.91730216053644));
#21813=CARTESIAN_POINT('Ctrl Pts',(90.3514486416872,-3.66640238856974,2.79737238413463));
#21814=CARTESIAN_POINT('Ctrl Pts',(90.4818372157755,-4.36367090710306,0.0395547452550024));
#21815=CARTESIAN_POINT('Ctrl Pts',(90.5470315028196,-4.03754750937051,-1.33429842360129));
#21816=CARTESIAN_POINT('Ctrl Pts',(90.5796286463417,-3.71907453321684,-1.94367293110128));
#21817=CARTESIAN_POINT('Ctrl Pts',(82.307855963792,2.29508936814274,-3.22291523290208));
#21818=CARTESIAN_POINT('Ctrl Pts',(82.3404984367184,2.82391607075853,-2.84634438165137));
#21819=CARTESIAN_POINT('Ctrl Pts',(82.4057380531669,3.68542102552352,-1.82995900702202));
#21820=CARTESIAN_POINT('Ctrl Pts',(82.5361719566594,4.27636686552807,0.787155484537778));
#21821=CARTESIAN_POINT('Ctrl Pts',(82.6991576742698,2.46089253457709,3.95029523024854));
#21822=CARTESIAN_POINT('Ctrl Pts',(82.8947405354022,-1.93078657401334,4.23713164316919));
#21823=CARTESIAN_POINT('Ctrl Pts',(83.0903233965346,-4.59301783545288,0.742911345620072));
#21824=CARTESIAN_POINT('Ctrl Pts',(83.2859062576669,-3.16664449183598,-3.41077393808554));
#21825=CARTESIAN_POINT('Ctrl Pts',(83.4814891187993,1.08370736165695,-4.52630115217425));
#21826=CARTESIAN_POINT('Ctrl Pts',(83.6770719799316,4.36730849980295,-1.60773529411797));
#21827=CARTESIAN_POINT('Ctrl Pts',(83.8726548410641,3.75961962752953,2.7432158448027));
#21828=CARTESIAN_POINT('Ctrl Pts',(84.0682377021964,-0.198592098039204,
4.64977843972425));
#21829=CARTESIAN_POINT('Ctrl Pts',(84.2638205633287,-3.97971242317383,2.41275617249475));
#21830=CARTESIAN_POINT('Ctrl Pts',(84.4594034244612,-4.21448928768466,-1.97428716112127));
#21831=CARTESIAN_POINT('Ctrl Pts',(84.6549862855934,-0.693619233453502,
-4.60202011225595));
#21832=CARTESIAN_POINT('Ctrl Pts',(84.8505691467259,3.44533478003599,-3.12879027541714));
#21833=CARTESIAN_POINT('Ctrl Pts',(85.0461520078582,4.51408748207532,1.13256445427651));
#21834=CARTESIAN_POINT('Ctrl Pts',(85.2417348689906,1.56024100329834,4.38466985540846));
#21835=CARTESIAN_POINT('Ctrl Pts',(85.437317730123,-2.78396647953264,3.72950521489826));
#21836=CARTESIAN_POINT('Ctrl Pts',(85.6329005912553,-4.64732528218793,-0.249097361775471));
#21837=CARTESIAN_POINT('Ctrl Pts',(85.8284834523878,-2.36935700885369,-4.00572442066759));
#21838=CARTESIAN_POINT('Ctrl Pts',(86.02406631352,2.01999358636394,-4.19276835036339));
#21839=CARTESIAN_POINT('Ctrl Pts',(86.2196491746525,4.60928665604361,-0.643550651485564));
#21840=CARTESIAN_POINT('Ctrl Pts',(86.4152320357848,3.09114999924119,3.47914823150234));
#21841=CARTESIAN_POINT('Ctrl Pts',(86.6108148969172,-1.18157364853143,4.50150690854415));
#21842=CARTESIAN_POINT('Ctrl Pts',(86.8063977580496,-4.40137287455832,1.512480656971));
#21843=CARTESIAN_POINT('Ctrl Pts',(87.0019806191819,-3.69901859323395,-2.82434806206138));
#21844=CARTESIAN_POINT('Ctrl Pts',(87.1975634803144,0.299606744969849,-4.6443424258021));
#21845=CARTESIAN_POINT('Ctrl Pts',(87.3931463414466,4.03124661214913,-2.3256681891755));
#21846=CARTESIAN_POINT('Ctrl Pts',(87.5887292025792,4.17055965039982,2.06545653780747));
#21847=CARTESIAN_POINT('Ctrl Pts',(87.7843120637113,0.593402587684435,4.61601073419793));
#21848=CARTESIAN_POINT('Ctrl Pts',(87.9798949248439,-3.51254961998634,3.05314316828636));
#21849=CARTESIAN_POINT('Ctrl Pts',(88.1754777859761,-4.48839298437938,-1.23044250245362));
#21850=CARTESIAN_POINT('Ctrl Pts',(88.3710606471085,-1.46454564443096,-4.41755620337796));
#21851=CARTESIAN_POINT('Ctrl Pts',(88.566643508241,2.8644049141729,-3.66809408797527));
#21852=CARTESIAN_POINT('Ctrl Pts',(88.7622263693732,4.64079170288519,0.350079547399718));
#21853=CARTESIAN_POINT('Ctrl Pts',(88.9578092305058,2.28174328173701,4.05629460914468));
#21854=CARTESIAN_POINT('Ctrl Pts',(89.1533920916379,-2.11075463879587,4.14785339298334));
#21855=CARTESIAN_POINT('Ctrl Pts',(89.3489749527706,-4.62202735051278,0.543193777132494));
#21856=CARTESIAN_POINT('Ctrl Pts',(89.5445578139026,-3.01510589170997,-3.54555499571779));
#21857=CARTESIAN_POINT('Ctrl Pts',(89.7401406750352,1.27984042209396,-4.47470945295592));
#21858=CARTESIAN_POINT('Ctrl Pts',(89.9357235361675,4.43184032895884,-1.41651735000079));
#21859=CARTESIAN_POINT('Ctrl Pts',(90.1313063972999,3.6395535853136,2.90428494737804));
#21860=CARTESIAN_POINT('Ctrl Pts',(90.3268892584322,-0.406317802387683,
4.63634881305585));
#21861=CARTESIAN_POINT('Ctrl Pts',(90.4898749760426,-3.45692003612324,2.63754264217168));
#21862=CARTESIAN_POINT('Ctrl Pts',(90.6202635501308,-4.11434965153871,0.0372947584318718));
#21863=CARTESIAN_POINT('Ctrl Pts',(90.6854578371749,-3.80685953223677,-1.25806239083166));
#21864=CARTESIAN_POINT('Ctrl Pts',(90.718054980697,-3.50658272256043,-1.83261987831497));
#21865=CARTESIAN_POINT('Ctrl Pts',(82.4462822981473,2.15601160097152,-3.0276130975709));
#21866=CARTESIAN_POINT('Ctrl Pts',(82.4789247710738,2.65279247650918,-2.67386167718884));
#21867=CARTESIAN_POINT('Ctrl Pts',(82.5441643875223,3.46209197593166,-1.71906719764665));
#21868=CARTESIAN_POINT('Ctrl Pts',(82.6745982910148,4.01722769495016,0.739455456501537));
#21869=CARTESIAN_POINT('Ctrl Pts',(82.8375840086252,2.3117674313423,3.71091534033396));
#21870=CARTESIAN_POINT('Ctrl Pts',(83.0331668697575,-1.81378481829728,3.98037004759811));
#21871=CARTESIAN_POINT('Ctrl Pts',(83.2287497308899,-4.31469025745127,0.697892422788916));
#21872=CARTESIAN_POINT('Ctrl Pts',(83.4243325920222,-2.97475224944107,-3.20408794571452));
#21873=CARTESIAN_POINT('Ctrl Pts',(83.6199154531546,1.01803689051175,-4.25201647004949));
#21874=CARTESIAN_POINT('Ctrl Pts',(83.815498314287,4.10265845038372,-1.51030979164646));
#21875=CARTESIAN_POINT('Ctrl Pts',(84.0110811754194,3.53179429294001,2.57698252079379));
#21876=CARTESIAN_POINT('Ctrl Pts',(84.2066640365517,-0.186557819132022,
4.3680112840683));
#21877=CARTESIAN_POINT('Ctrl Pts',(84.4022468976841,-3.73854991095039,2.26654803530542));
#21878=CARTESIAN_POINT('Ctrl Pts',(84.5978297588165,-3.95909977299548,-1.85464935793378));
#21879=CARTESIAN_POINT('Ctrl Pts',(84.7934126199488,-0.651587312782014,
-4.32314701451353));
#21880=CARTESIAN_POINT('Ctrl Pts',(84.9889954810813,3.23655447064327,-2.93919192186622));
#21881=CARTESIAN_POINT('Ctrl Pts',(85.1845783422135,4.24054292362064,1.06393334227509));
#21882=CARTESIAN_POINT('Ctrl Pts',(85.380161203346,1.46569355865423,4.11896774300371));
#21883=CARTESIAN_POINT('Ctrl Pts',(85.5757440644783,-2.61526374959657,3.50350475271963));
#21884=CARTESIAN_POINT('Ctrl Pts',(85.7713269256107,-4.36570678291,-0.234002566180649));
#21885=CARTESIAN_POINT('Ctrl Pts',(85.966909786743,-2.22577877307914,-3.76298563408145));
#21886=CARTESIAN_POINT('Ctrl Pts',(86.1624926478755,1.89758606638183,-3.93869508048168));
#21887=CARTESIAN_POINT('Ctrl Pts',(86.3580755090077,4.32997322046552,-0.604552785471028));
#21888=CARTESIAN_POINT('Ctrl Pts',(86.5536583701403,2.90383257018886,3.26831889543747));
#21889=CARTESIAN_POINT('Ctrl Pts',(86.7492412312724,-1.10997267862275,4.22872470736441));
#21890=CARTESIAN_POINT('Ctrl Pts',(86.944824092405,-4.13465859302386,1.42082739257919));
#21891=CARTESIAN_POINT('Ctrl Pts',(87.1404069535373,-3.47486555857972,-2.65319829001405));
#21892=CARTESIAN_POINT('Ctrl Pts',(87.3359898146697,0.281451183056565,-4.36290468157959));
#21893=CARTESIAN_POINT('Ctrl Pts',(87.5315726758021,3.78696123245258,-2.18473740738487));
#21894=CARTESIAN_POINT('Ctrl Pts',(87.7271555369346,3.91783218275379,1.9402940550498));
#21895=CARTESIAN_POINT('Ctrl Pts',(87.9227383980667,0.557443592764954,4.33628983310282));
#21896=CARTESIAN_POINT('Ctrl Pts',(88.1183212591992,-3.29969622743145,2.8681288762098));
#21897=CARTESIAN_POINT('Ctrl Pts',(88.3139041203315,-4.21640546044272,-1.15588017897761));
#21898=CARTESIAN_POINT('Ctrl Pts',(88.5094869814639,-1.37579714471017,-4.14986124489519));
#21899=CARTESIAN_POINT('Ctrl Pts',(88.7050698425962,2.69082777801989,-3.44581501570436));
#21900=CARTESIAN_POINT('Ctrl Pts',(88.9006527037287,4.3595691252797,0.328865435888209));
#21901=CARTESIAN_POINT('Ctrl Pts',(89.096235564861,2.14347426037042,3.8104913715631));
#21902=CARTESIAN_POINT('Ctrl Pts',(89.2918184259934,-1.98284718286635,3.89650187854686));
#21903=CARTESIAN_POINT('Ctrl Pts',(89.4874012871258,-4.34194185465522,0.510277334438133));
#21904=CARTESIAN_POINT('Ctrl Pts',(89.6829841482581,-2.83239658155217,-3.33070154424358));
#21905=CARTESIAN_POINT('Ctrl Pts',(89.8785670093905,1.20228468473967,-4.20355112330852));
#21906=CARTESIAN_POINT('Ctrl Pts',(90.0741498705228,4.16327978139733,-1.3306792676446));
#21907=CARTESIAN_POINT('Ctrl Pts',(90.2697327316552,3.41900400969726,2.72829116198692));
#21908=CARTESIAN_POINT('Ctrl Pts',(90.4653155927876,-0.381695766530438,
4.35539546557527));
#21909=CARTESIAN_POINT('Ctrl Pts',(90.6283013103979,-3.24743768367674,2.47771290020874));
#21910=CARTESIAN_POINT('Ctrl Pts',(90.7586898844862,-3.86502839597435,0.035034771608743));
#21911=CARTESIAN_POINT('Ctrl Pts',(90.8238841715303,-3.57617155510303,-1.18182635806204));
#21912=CARTESIAN_POINT('Ctrl Pts',(90.8564813150523,-3.29409091190402,-1.72156682552866));
#21913=CARTESIAN_POINT('Ctrl Pts',(90.4430005297901,0.0295740726440573,
3.72695441077288));
#21914=CARTESIAN_POINT('Ctrl Pts',(90.4430005297901,-0.0884458352819757,
3.73973311544785));
#21915=CARTESIAN_POINT('Ctrl Pts',(90.4430005297901,-0.206685143677292,
3.74654596528331));
#21916=CARTESIAN_POINT('Ctrl Pts',(90.4430005297901,-0.324736322595996,
3.74724091818273));
#21917=CARTESIAN_POINT('Ctrl Pts',(90.4430005297901,-0.439404897079654,
3.7479159581022));
#21918=CARTESIAN_POINT('Ctrl Pts',(90.4430005297901,-0.553896885543204,
3.74281974148777));
#21919=CARTESIAN_POINT('Ctrl Pts',(90.4430005297901,-0.66791598104826,3.73223833786101));
#21920=CARTESIAN_POINT('Ctrl Pts',(90.4430005297901,-0.783952175660468,
3.72146973980235));
#21921=CARTESIAN_POINT('Ctrl Pts',(90.4430005297901,-0.899499226843573,
3.7050200613725));
#21922=CARTESIAN_POINT('Ctrl Pts',(90.4430005297901,-1.01425304689082,3.68313712188346));
#21923=CARTESIAN_POINT('Ctrl Pts',(90.4430005297901,-1.13104622386595,3.66086528793991));
#21924=CARTESIAN_POINT('Ctrl Pts',(90.4430005297901,-1.24701846212934,3.63296523737056));
#21925=CARTESIAN_POINT('Ctrl Pts',(90.4430005297901,-1.36184717318808,3.59964481501033));
#21926=CARTESIAN_POINT('Ctrl Pts',(90.4430005297901,-1.37934384898826,3.59456771693801));
#21927=CARTESIAN_POINT('Ctrl Pts',(90.4430005297901,-1.39681395895273,3.58936467583838));
#21928=CARTESIAN_POINT('Ctrl Pts',(90.4430005297901,-1.41425634058431,3.584036323652));
#21929=CARTESIAN_POINT('Ctrl Pts',(90.4430005297901,-1.43024624853253,3.57915167757697));
#21930=CARTESIAN_POINT('Ctrl Pts',(90.4430005297901,-1.44620373585888,3.57416449842206));
#21931=CARTESIAN_POINT('Ctrl Pts',(90.4430005297901,-1.46212623027145,3.56907619712215));
#21932=CARTESIAN_POINT('Ctrl Pts',(90.4430005297901,-1.57729676935156,3.53227151134062));
#21933=CARTESIAN_POINT('Ctrl Pts',(90.4430005297901,-1.6906653553074,3.4901716855535));
#21934=CARTESIAN_POINT('Ctrl Pts',(90.4430005297901,-1.8019109939639,3.44308149795093));
#21935=CARTESIAN_POINT('Ctrl Pts',(90.4430005297901,-1.91505125573011,3.39518931793994));
#21936=CARTESIAN_POINT('Ctrl Pts',(90.4430005297901,-2.02599639340762,3.34213517090997));
#21937=CARTESIAN_POINT('Ctrl Pts',(90.4430005297901,-2.13440929064491,3.28418473248124));
#21938=CARTESIAN_POINT('Ctrl Pts',(90.4430005297901,-2.24357700600436,3.22583081769288));
#21939=CARTESIAN_POINT('Ctrl Pts',(90.4430005297901,-2.35017791442109,3.16251190946834));
#21940=CARTESIAN_POINT('Ctrl Pts',(90.4430005297901,-2.45385647085219,3.09444766228528));
#21941=CARTESIAN_POINT('Ctrl Pts',(90.4430005297901,-2.51004735209134,3.05755874174328));
#21942=CARTESIAN_POINT('Ctrl Pts',(90.4430005297901,-2.56537957209502,3.01927509056427));
#21943=CARTESIAN_POINT('Ctrl Pts',(90.4430005297901,-2.61979383101806,2.97962587081534));
#21944=CARTESIAN_POINT('Ctrl Pts',(90.4430005297901,-2.6583589385645,2.95152521385496));
#21945=CARTESIAN_POINT('Ctrl Pts',(90.4430005297901,-2.69646291239529,2.92273854683793));
#21946=CARTESIAN_POINT('Ctrl Pts',(90.4430005297901,-2.73408385528245,2.89327509668863));
#21947=CARTESIAN_POINT('Ctrl Pts',(90.4430005297901,-2.75355183901951,2.87802843022242));
#21948=CARTESIAN_POINT('Ctrl Pts',(90.4430005297901,-2.77289124006853,2.86259967027211));
#21949=CARTESIAN_POINT('Ctrl Pts',(90.4430005297901,-2.79207491946629,2.84701017273444));
#21950=CARTESIAN_POINT('Ctrl Pts',(90.4430005297901,-2.89080728506944,2.76677593098424));
#21951=CARTESIAN_POINT('Ctrl Pts',(90.4430005297901,-2.98557254574996,2.68216713774138));
#21952=CARTESIAN_POINT('Ctrl Pts',(90.4430005297901,-3.0760218382525,2.59346212800552));
#21953=CARTESIAN_POINT('Ctrl Pts',(90.4430005297901,-3.16657121142245,2.5046589676227));
#21954=CARTESIAN_POINT('Ctrl Pts',(90.4430005297901,-3.25279589353019,2.41175014113957));
#21955=CARTESIAN_POINT('Ctrl Pts',(90.4430005297901,-3.33432693640993,2.31496642130862));
#21956=CARTESIAN_POINT('Ctrl Pts',(90.4430005297901,-3.41466240181752,2.21960194537565));
#21957=CARTESIAN_POINT('Ctrl Pts',(90.4430005297901,-3.49044160687377,2.1204749177954));
#21958=CARTESIAN_POINT('Ctrl Pts',(90.4430005297901,-3.56128171283007,2.01776553973377));
#21959=CARTESIAN_POINT('Ctrl Pts',(90.4430005297901,-3.57213897168619,2.0020238593747));
#21960=CARTESIAN_POINT('Ctrl Pts',(90.4430005297901,-3.58288014117297,1.98619795895379));
#21961=CARTESIAN_POINT('Ctrl Pts',(90.4430005297901,-3.5935037628077,1.97028841204376));
#21962=CARTESIAN_POINT('Ctrl Pts',(90.4430005297901,-3.65258853086704,1.88180522604296));
#21963=CARTESIAN_POINT('Ctrl Pts',(90.4430005297901,-3.70803921479688,1.79073595284717));
#21964=CARTESIAN_POINT('Ctrl Pts',(90.4430005297901,-3.75982007731666,1.69733475008557));
#21965=CARTESIAN_POINT('Ctrl Pts',(90.4430005297901,-3.76811332474678,1.68237556927863));
#21966=CARTESIAN_POINT('Ctrl Pts',(90.4430005297901,-3.77631159693478,1.66735785530935));
#21967=CARTESIAN_POINT('Ctrl Pts',(90.4430005297901,-3.78440902583728,1.65229362110775));
#21968=CARTESIAN_POINT('Ctrl Pts',(90.4430005297901,-3.84295084533117,1.54338402893199));
#21969=CARTESIAN_POINT('Ctrl Pts',(90.4430005297901,-3.89630994738891,1.43189315586789));
#21970=CARTESIAN_POINT('Ctrl Pts',(90.4430005297901,-3.94451322877546,1.318276879715));
#21971=CARTESIAN_POINT('Ctrl Pts',(90.4430005297901,-3.99420842084563,1.20114413473779));
#21972=CARTESIAN_POINT('Ctrl Pts',(90.4430005297901,-4.03842411533983,1.08175183814539));
#21973=CARTESIAN_POINT('Ctrl Pts',(90.4430005297901,-4.07715067449774,0.960560639470474));
#21974=CARTESIAN_POINT('Ctrl Pts',(90.4430005297901,-4.11629615156748,0.83805847578899));
#21975=CARTESIAN_POINT('Ctrl Pts',(90.4430005297901,-4.14983341986074,0.713717519612734));
#21976=CARTESIAN_POINT('Ctrl Pts',(90.4430005297901,-4.17770772803754,0.587984615666701));
#21977=CARTESIAN_POINT('Ctrl Pts',(90.4430005297901,-4.20559840491458,0.462177877270582));
#21978=CARTESIAN_POINT('Ctrl Pts',(90.4430005297901,-4.22781973772143,0.334976713975839));
#21979=CARTESIAN_POINT('Ctrl Pts',(90.4430005297901,-4.24426791493627,0.206812112669376));
#21980=CARTESIAN_POINT('Ctrl Pts',(90.4430005297901,-4.24661469917405,0.18852591218294));
#21981=CARTESIAN_POINT('Ctrl Pts',(90.4430005297901,-4.24884387475331,0.170220083948819));
#21982=CARTESIAN_POINT('Ctrl Pts',(90.4430005297901,-4.250955053885,0.151895867868593));
#21983=CARTESIAN_POINT('Ctrl Pts',(90.4430005297901,-4.25302188555422,0.133956570563174));
#21984=CARTESIAN_POINT('Ctrl Pts',(90.4430005297901,-4.25497512784509,0.116003677579542));
#21985=CARTESIAN_POINT('Ctrl Pts',(90.4430005297901,-4.25681383615619,0.0980463316274623));
#21986=CARTESIAN_POINT('Ctrl Pts',(90.4430005297901,-4.25874402274224,0.0791955829424459));
#21987=CARTESIAN_POINT('Ctrl Pts',(90.4430005297901,-4.26054829999988,0.060337316736268));
#21988=CARTESIAN_POINT('Ctrl Pts',(90.4430005297901,-4.26222661848669,0.0414729768254014));
#21989=CARTESIAN_POINT('Ctrl Pts',(90.4430005297901,-4.27381294533361,-0.0887576138975155));
#21990=CARTESIAN_POINT('Ctrl Pts',(90.4430005297901,-4.27940028200127,-0.219276168333582));
#21991=CARTESIAN_POINT('Ctrl Pts',(90.4430005297901,-4.27910474674529,-0.349707946362895));
#21992=CARTESIAN_POINT('Ctrl Pts',(90.4430005297901,-4.27880600451492,-0.481555093161264));
#21993=CARTESIAN_POINT('Ctrl Pts',(90.4430005297901,-4.27249612571316,-0.613314293186454));
#21994=CARTESIAN_POINT('Ctrl Pts',(90.4430005297901,-4.26024353120833,-0.744611026749141));
#21995=CARTESIAN_POINT('Ctrl Pts',(90.4430005297901,-4.25441728433827,-0.807044104304067));
#21996=CARTESIAN_POINT('Ctrl Pts',(90.4430005297901,-4.24724656795236,-0.869372726950488));
#21997=CARTESIAN_POINT('Ctrl Pts',(90.4430005297901,-4.23873461501024,-0.931556866122163));
#21998=CARTESIAN_POINT('Ctrl Pts',(90.4430005297901,-4.23512308808359,-0.95794090449223));
#21999=CARTESIAN_POINT('Ctrl Pts',(90.4430005297901,-4.23126959330347,-0.984301416906839));
#22000=CARTESIAN_POINT('Ctrl Pts',(90.4430005297901,-4.22717812966963,-1.01061216318249));
#22001=CARTESIAN_POINT('Ctrl Pts',(90.4430005297901,-4.2065986047243,-1.14295176283902));
#22002=CARTESIAN_POINT('Ctrl Pts',(90.4430005297901,-4.17998717842944,-1.27415495162273));
#22003=CARTESIAN_POINT('Ctrl Pts',(90.4430005297901,-4.14743840993115,-1.40383584322983));
#22004=CARTESIAN_POINT('Ctrl Pts',(90.4430005297901,-4.11495992046892,-1.5332367289111));
#22005=CARTESIAN_POINT('Ctrl Pts',(90.4430005297901,-4.0765696800258,-1.66112266042091));
#22006=CARTESIAN_POINT('Ctrl Pts',(90.4430005297901,-4.03231018303459,-1.78711174601695));
#22007=CARTESIAN_POINT('Ctrl Pts',(90.4430005297901,-4.00078732768196,-1.87684470710418));
#22008=CARTESIAN_POINT('Ctrl Pts',(90.4430005297901,-3.96628611270671,-1.96561551665267));
#22009=CARTESIAN_POINT('Ctrl Pts',(90.4430005297901,-3.92880598357854,-2.05328335682083));
#22010=CARTESIAN_POINT('Ctrl Pts',(82.4430005297902,1.9774016913413,3.97328893098977));
#22011=CARTESIAN_POINT('Ctrl Pts',(82.4430005297901,2.09010205945685,3.90686165204003));
#22012=CARTESIAN_POINT('Ctrl Pts',(82.4430005297901,2.1994288641269,3.83533535974094));
#22013=CARTESIAN_POINT('Ctrl Pts',(82.4430005297901,2.30496647500185,3.75870816478726));
#22014=CARTESIAN_POINT('Ctrl Pts',(82.4430005297901,2.31220701604365,3.75345105933091));
#22015=CARTESIAN_POINT('Ctrl Pts',(82.4430005297901,2.31942970874689,3.74816992928515));
#22016=CARTESIAN_POINT('Ctrl Pts',(82.4430005297901,2.32663441280679,3.74286476721894));
#22017=CARTESIAN_POINT('Ctrl Pts',(82.4430005297901,2.43415121558717,3.66369509434307));
#22018=CARTESIAN_POINT('Ctrl Pts',(82.4430005297901,2.53766541991209,3.57917623912721));
#22019=CARTESIAN_POINT('Ctrl Pts',(82.4430005297901,2.63699553330001,3.48971947438876));
#22020=CARTESIAN_POINT('Ctrl Pts',(82.4430005297901,2.69497714530243,3.43750119689823));
#22021=CARTESIAN_POINT('Ctrl Pts',(82.4430005297901,2.75153231248618,3.38359974223897));
#22022=CARTESIAN_POINT('Ctrl Pts',(82.4430005297901,2.80661797434521,3.32809262431144));
#22023=CARTESIAN_POINT('Ctrl Pts',(82.4430005297901,2.82333285684607,3.31124985755857));
#22024=CARTESIAN_POINT('Ctrl Pts',(82.4430005297901,2.83991240093079,3.29425923599673));
#22025=CARTESIAN_POINT('Ctrl Pts',(82.4430005297901,2.85635530402485,3.2771228831448));
#22026=CARTESIAN_POINT('Ctrl Pts',(82.4430005297901,2.87182248494779,3.26100340178533));
#22027=CARTESIAN_POINT('Ctrl Pts',(82.4430005297901,2.88716274481627,3.24476121188179));
#22028=CARTESIAN_POINT('Ctrl Pts',(82.4430005297901,2.9023727429123,3.22840114134904));
#22029=CARTESIAN_POINT('Ctrl Pts',(82.4430005297901,2.99230521077527,3.1316686165891));
#22030=CARTESIAN_POINT('Ctrl Pts',(82.4430005297901,3.07771715590702,3.03078619893305));
#22031=CARTESIAN_POINT('Ctrl Pts',(82.4430005297901,3.15844240805742,2.92616122323708));
#22032=CARTESIAN_POINT('Ctrl Pts',(82.4430005297901,3.2395838873707,2.82099679110536));
#22033=CARTESIAN_POINT('Ctrl Pts',(82.4430005297901,3.31599056868566,2.71205028408578));
#22034=CARTESIAN_POINT('Ctrl Pts',(82.4430005297901,3.3874469961184,2.59971212324649));
#22035=CARTESIAN_POINT('Ctrl Pts',(82.4430005297901,3.41263912962364,2.56010703736026));
#22036=CARTESIAN_POINT('Ctrl Pts',(82.4430005297901,3.43721553345861,2.52008024072263));
#22037=CARTESIAN_POINT('Ctrl Pts',(82.4430005297901,3.46116526677622,2.47964845206219));
#22038=CARTESIAN_POINT('Ctrl Pts',(82.4430005297901,3.47596320889565,2.45466665955337));
#22039=CARTESIAN_POINT('Ctrl Pts',(82.4430005297901,3.4905218915381,2.42953025043779));
#22040=CARTESIAN_POINT('Ctrl Pts',(82.4430005297901,3.50483857765273,2.4042431483245));
#22041=CARTESIAN_POINT('Ctrl Pts',(82.4430005297901,3.51750213823568,2.3818759086564));
#22042=CARTESIAN_POINT('Ctrl Pts',(82.4430005297901,3.52997604592584,2.35939102284286));
#22043=CARTESIAN_POINT('Ctrl Pts',(82.4430005297901,3.54224655904972,2.33681381979864));
#22044=CARTESIAN_POINT('Ctrl Pts',(82.4430005297901,3.60511418791248,2.22114015502084));
#22045=CARTESIAN_POINT('Ctrl Pts',(82.4430005297901,3.66273152318934,2.10289696968469));
#22046=CARTESIAN_POINT('Ctrl Pts',(82.4430005297901,3.71493478777603,1.98247901087182));
#22047=CARTESIAN_POINT('Ctrl Pts',(82.4430005297901,3.7664679243965,1.86360684507541));
#22048=CARTESIAN_POINT('Ctrl Pts',(82.4430005297901,3.81272526802198,1.74261452974662));
#22049=CARTESIAN_POINT('Ctrl Pts',(82.4430005297901,3.85350025988324,1.61986682033174));
#22050=CARTESIAN_POINT('Ctrl Pts',(82.4430005297901,3.89507059812238,1.49472482604712));
#22051=CARTESIAN_POINT('Ctrl Pts',(82.4430005297901,3.9309430977877,1.36775746124));
#22052=CARTESIAN_POINT('Ctrl Pts',(82.4430005297901,3.96084235932242,1.2393481640155));
#22053=CARTESIAN_POINT('Ctrl Pts',(82.4430005297901,3.98903875393377,1.11825222282973));
#22054=CARTESIAN_POINT('Ctrl Pts',(82.4430005297901,4.01192267483145,0.99587330142771));
#22055=CARTESIAN_POINT('Ctrl Pts',(82.4430005297901,4.02921301288842,0.872540673797174));
#22056=CARTESIAN_POINT('Ctrl Pts',(82.4430005297901,4.03025722954013,0.865092237390287));
#22057=CARTESIAN_POINT('Ctrl Pts',(82.4430005297901,4.0312810292029,0.85764032654507));
#22058=CARTESIAN_POINT('Ctrl Pts',(82.4430005297901,4.03228434397425,0.850185015481214));
#22059=CARTESIAN_POINT('Ctrl Pts',(82.4430005297901,4.03459129039469,0.83304283471883));
#22060=CARTESIAN_POINT('Ctrl Pts',(82.4430005297901,4.03678865170643,0.81589217044497));
#22061=CARTESIAN_POINT('Ctrl Pts',(82.4430005297901,4.03887577431093,0.798735610694986));
#22062=CARTESIAN_POINT('Ctrl Pts',(82.4430005297901,4.05392301973049,0.675044283430583));
#22063=CARTESIAN_POINT('Ctrl Pts',(82.4430005297901,4.06324834973385,0.551017529409657));
#22064=CARTESIAN_POINT('Ctrl Pts',(82.4430005297901,4.06666460622878,0.426983323700702));
#22065=CARTESIAN_POINT('Ctrl Pts',(82.4430005297901,4.06939901272037,0.327705082218145));
#22066=CARTESIAN_POINT('Ctrl Pts',(82.4430005297901,4.06834683332187,0.228421806362535));
#22067=CARTESIAN_POINT('Ctrl Pts',(82.4430005297901,4.06338801735055,0.129303333680082));
#22068=CARTESIAN_POINT('Ctrl Pts',(82.4430005297901,4.05712578276322,0.00413169362238594));
#22069=CARTESIAN_POINT('Ctrl Pts',(82.4430005297901,4.04463442778872,-0.120778201880177));
#22070=CARTESIAN_POINT('Ctrl Pts',(82.4430005297901,4.02608868523045,-0.244998516667174));
#22071=CARTESIAN_POINT('Ctrl Pts',(82.4430005297901,4.00761010244444,-0.368768991927616));
#22072=CARTESIAN_POINT('Ctrl Pts',(82.4430005297901,3.98312043438457,-0.491855671889886));
#22073=CARTESIAN_POINT('Ctrl Pts',(82.4430005297901,3.95274824392976,-0.613809207916153));
#22074=CARTESIAN_POINT('Ctrl Pts',(82.4430005297901,3.94615948295374,-0.640265077151297));
#22075=CARTESIAN_POINT('Ctrl Pts',(82.4430005297901,3.93929375074547,-0.666667446927112));
#22076=CARTESIAN_POINT('Ctrl Pts',(82.4430005297901,3.93215207449842,-0.693011663701303));
#22077=CARTESIAN_POINT('Ctrl Pts',(82.4430005297901,3.92670631144765,-0.713099995536515));
#22078=CARTESIAN_POINT('Ctrl Pts',(82.4430005297901,3.92110068729186,-0.733151964085459));
#22079=CARTESIAN_POINT('Ctrl Pts',(82.4430005297901,3.9153411470454,-0.753147780879801));
#22080=CARTESIAN_POINT('Ctrl Pts',(82.4430005297901,3.88128865297465,-0.871370313181259));
#22081=CARTESIAN_POINT('Ctrl Pts',(82.4430005297901,3.84181409822679,-0.987802709833606));
#22082=CARTESIAN_POINT('Ctrl Pts',(82.4430005297901,3.79712203089279,-1.10205584095973));
#22083=CARTESIAN_POINT('Ctrl Pts',(82.4430005297901,3.75260677405727,-1.21585696450885));
#22084=CARTESIAN_POINT('Ctrl Pts',(82.4430005297901,3.70291471512788,-1.32749679081321));
#22085=CARTESIAN_POINT('Ctrl Pts',(82.4430005297901,3.6482030112339,-1.43656648416229));
#22086=CARTESIAN_POINT('Ctrl Pts',(82.4430005297901,3.59845450992584,-1.5357418597412));
#22087=CARTESIAN_POINT('Ctrl Pts',(82.4430005297901,3.54455500137787,-1.63279237552513));
#22088=CARTESIAN_POINT('Ctrl Pts',(82.4430005297901,3.48659512784045,-1.72738526130349));
#22089=CARTESIAN_POINT('Ctrl Pts',(82.4430005297901,3.42673021387979,-1.82508725102155));
#22090=CARTESIAN_POINT('Ctrl Pts',(82.4430005297901,3.36253323060098,-1.92016776201095));
#22091=CARTESIAN_POINT('Ctrl Pts',(82.4430005297901,3.29416366019009,-2.01234893030668));
#22092=CARTESIAN_POINT('Ctrl Pts',(82.4430005297901,3.28199925485566,-2.02874992695784));
#22093=CARTESIAN_POINT('Ctrl Pts',(82.4430005297901,3.26970271301344,-2.04505905011743));
#22094=CARTESIAN_POINT('Ctrl Pts',(82.4430005297901,3.25727487268005,-2.06127461217243));
#22095=CARTESIAN_POINT('Ctrl Pts',(82.4430005297901,3.24649498934229,-2.07533995760012));
#22096=CARTESIAN_POINT('Ctrl Pts',(82.4430005297901,3.23562112293146,-2.08932859706152));
#22097=CARTESIAN_POINT('Ctrl Pts',(82.4430005297901,3.22465780066578,-2.10323500148988));
#22098=CARTESIAN_POINT('Ctrl Pts',(82.4430005297901,3.15047393396632,-2.19733338037383));
#22099=CARTESIAN_POINT('Ctrl Pts',(82.4430005297901,3.07214423094065,-2.28773884705976));
#22100=CARTESIAN_POINT('Ctrl Pts',(82.4430005297901,2.98991394061097,-2.37420105586575));
#22101=CARTESIAN_POINT('Ctrl Pts',(82.4430005297901,2.90806315296147,-2.46026423117879));
#22102=CARTESIAN_POINT('Ctrl Pts',(82.4430005297901,2.82234707694838,-2.54242092981904));
#22103=CARTESIAN_POINT('Ctrl Pts',(82.4430005297901,2.73297569134897,-2.62038408617641));
#22104=CARTESIAN_POINT('Ctrl Pts',(82.4430005297901,2.64463815606218,-2.69744536288816));
#22105=CARTESIAN_POINT('Ctrl Pts',(82.4430005297901,2.55272879793543,-2.77040993934337));
#22106=CARTESIAN_POINT('Ctrl Pts',(82.4430005297901,2.45742821326915,-2.83895504479805));
#22107=CARTESIAN_POINT('Ctrl Pts',(82.4430005297901,2.36212762860286,-2.90750015025273));
#22108=CARTESIAN_POINT('Ctrl Pts',(82.4430005297901,2.26343528680515,-2.97162624539521));
#22109=CARTESIAN_POINT('Ctrl Pts',(82.4430005297901,2.16151778945159,-3.03095833168066));
#22110=CARTESIAN_POINT('Origin',(81.4430005297901,0.,0.));
#22111=CARTESIAN_POINT('',(82.4430005297901,-5.42440960677665,-6.64298586220318E-16));
#22112=CARTESIAN_POINT('Origin',(82.4430005297901,0.,0.));
#22113=CARTESIAN_POINT('',(81.4430005297901,-5.42440960677665,-6.64298586220318E-16));
#22114=CARTESIAN_POINT('',(81.4430005297901,-5.42440960677665,-6.64298586220318E-16));
#22115=CARTESIAN_POINT('Origin',(81.4430005297901,0.,0.));
#22116=CARTESIAN_POINT('Origin',(82.4430005297901,0.,0.));
#22117=CARTESIAN_POINT('Origin',(90.4430005297901,0.,0.));
#22118=CARTESIAN_POINT('Origin',(81.4430005297901,0.,0.));
#22119=CARTESIAN_POINT('',(0.,0.,0.));
#22120=CARTESIAN_POINT('Origin',(30.1110679337117,0.,0.));
#22121=CARTESIAN_POINT('',(30.4110679337117,-7.4816555742545E-16,6.10923539706593));
#22122=CARTESIAN_POINT('Origin',(30.4110679337117,0.,0.));
#22123=CARTESIAN_POINT('',(30.1109792509259,-7.84904959794637E-16,6.4092353839582));
#22124=CARTESIAN_POINT('Origin',(30.1110679337117,-7.4816555742545E-16,
6.10923539706593));
#22125=CARTESIAN_POINT('Origin',(30.1109792509259,-7.84904959794637E-16,
0.));
#22126=CARTESIAN_POINT('Origin',(29.5420239984498,0.,0.));
#22127=CARTESIAN_POINT('',(28.9728913804021,-7.84863759081066E-16,6.40889895460077));
#22128=CARTESIAN_POINT('',(29.5420239984498,-7.84884362648318E-16,6.40906719549494));
#22129=CARTESIAN_POINT('Origin',(28.9728913804021,-7.84863759081066E-16,
0.));
#22130=CARTESIAN_POINT('Origin',(30.4110679337117,0.,0.));
#22131=CARTESIAN_POINT('Origin',(28.9729800631879,0.,0.));
#22132=CARTESIAN_POINT('',(28.6729800631879,-7.48124356711879E-16,6.1088989677085));
#22133=CARTESIAN_POINT('Origin',(28.9729800631879,-7.48124356711878E-16,
6.1088989677085));
#22134=CARTESIAN_POINT('Origin',(28.6729800631879,0.,0.));
#22135=CARTESIAN_POINT('Origin',(28.6729800631879,0.,-6.40881029802658));
#22136=CARTESIAN_POINT('',(0.,0.,0.));
#22137=CARTESIAN_POINT('Origin',(24.2263990006525,0.,0.));
#22138=CARTESIAN_POINT('',(24.5263990006525,-7.47952522416948E-16,6.1074958342087));
#22139=CARTESIAN_POINT('Origin',(24.5263990006525,0.,0.));
#22140=CARTESIAN_POINT('',(24.2263103178667,-7.84691924786135E-16,6.40749582110097));
#22141=CARTESIAN_POINT('Origin',(24.2263990006525,-7.47952522416948E-16,
6.1074958342087));
#22142=CARTESIAN_POINT('Origin',(24.2263103178667,-7.84691924786135E-16,
0.));
#22143=CARTESIAN_POINT('Origin',(23.6497386319918,0.,0.));
#22144=CARTESIAN_POINT('',(23.0729895805454,-7.84650172616918E-16,6.40715488876647));
#22145=CARTESIAN_POINT('',(23.6497386319918,-7.84671051911994E-16,6.40732538114918));
#22146=CARTESIAN_POINT('Origin',(23.0729895805454,-7.84650172616918E-16,
0.));
#22147=CARTESIAN_POINT('Origin',(24.5263990006525,0.,0.));
#22148=CARTESIAN_POINT('Origin',(23.0730782633312,0.,0.));
#22149=CARTESIAN_POINT('',(22.7730782633312,-7.47910770247731E-16,6.1071549018742));
#22150=CARTESIAN_POINT('Origin',(23.0730782633312,-7.47910770247731E-16,
6.1071549018742));
#22151=CARTESIAN_POINT('Origin',(22.7730782633312,0.,0.));
#22152=CARTESIAN_POINT('Origin',(22.7730782633312,0.,-6.40706623219228));
#22153=CARTESIAN_POINT('',(0.,0.,0.));
#22154=CARTESIAN_POINT('Origin',(3.02384907614375,-2.84862442585767,-2.80808455720391));
#22155=CARTESIAN_POINT('',(11.0238443243108,-2.84858103864746,-1.7782820253861));
#22156=CARTESIAN_POINT('',(10.9314356691441,-2.84862442585767,-1.5071351773836));
#22157=CARTESIAN_POINT('Ctrl Pts',(11.0238395724777,-2.84862442585767,-1.77821291115482));
#22158=CARTESIAN_POINT('Ctrl Pts',(11.023058671384,-2.84862442585767,-1.77602158816867));
#22159=CARTESIAN_POINT('Ctrl Pts',(11.0222784621947,-2.84862442585824,-1.7738300165061));
#22160=CARTESIAN_POINT('Ctrl Pts',(11.0062774820837,-2.84862442585824,-1.72883879945583));
#22161=CARTESIAN_POINT('Ctrl Pts',(10.9913133628153,-2.84862442585851,-1.68592261376175));
#22162=CARTESIAN_POINT('Ctrl Pts',(10.9612482690896,-2.84862442585851,-1.59778423981652));
#22163=CARTESIAN_POINT('Ctrl Pts',(10.9461611622631,-2.84862442585767,-1.55250504487283));
#22164=CARTESIAN_POINT('Ctrl Pts',(10.9314356691441,-2.84862442585767,-1.5071351773836));
#22165=CARTESIAN_POINT('',(11.0238490787776,-2.84862442708806,2.51132611227744));
#22166=CARTESIAN_POINT('',(11.0238490761438,-2.84862442585767,6.75363122348402));
#22167=CARTESIAN_POINT('',(10.7378093816896,-2.84862442585767,1.50713517738359));
#22168=CARTESIAN_POINT('Ctrl Pts',(10.7378093816896,-2.84862442585767,1.5071351773836));
#22169=CARTESIAN_POINT('Ctrl Pts',(10.7745509100274,-2.84862442585767,1.67768015510688));
#22170=CARTESIAN_POINT('Ctrl Pts',(10.8181799183082,-2.84862442695797,1.84746530235002));
#22171=CARTESIAN_POINT('Ctrl Pts',(10.9144539328214,-2.84862442695797,2.18146463191032));
#22172=CARTESIAN_POINT('Ctrl Pts',(10.9675731917165,-2.84862442585767,2.34753476778138));
#22173=CARTESIAN_POINT('Ctrl Pts',(11.0238490840452,-2.84862442585767,2.51132611046758));
#22174=CARTESIAN_POINT('',(10.4912624831434,-2.84862442585767,1.50713517738358));
#22175=CARTESIAN_POINT('',(13.3346225254169,-2.84862442585767,1.50713517738359));
#22176=CARTESIAN_POINT('',(10.0266594217773,-2.84681894361813,2.71028906402779));
#22177=CARTESIAN_POINT('Ctrl Pts',(10.0267941012523,-2.84862442585767,2.70859765771964));
#22178=CARTESIAN_POINT('Ctrl Pts',(10.0337979544476,-2.84862442585767,2.69250499494907));
#22179=CARTESIAN_POINT('Ctrl Pts',(10.0407818720682,-2.84862442585767,2.67640214955592));
#22180=CARTESIAN_POINT('Ctrl Pts',(10.1253566086339,-2.84862442585767,2.48069385236447));
#22181=CARTESIAN_POINT('Ctrl Pts',(10.2012319741895,-2.84862442733188,2.29789169628234));
#22182=CARTESIAN_POINT('Ctrl Pts',(10.3504646709377,-2.84862442733188,1.91583275087761));
#22183=CARTESIAN_POINT('Ctrl Pts',(10.4249778185909,-2.84862442585767,1.7113610340671));
#22184=CARTESIAN_POINT('Ctrl Pts',(10.4912624831434,-2.84862442585767,1.5071351773836));
#22185=CARTESIAN_POINT('',(9.84333237813747,-2.84681996992431,2.71028970229123));
#22186=CARTESIAN_POINT('',(11.0238490761438,-2.84862442585767,2.71179421793157));
#22187=CARTESIAN_POINT('',(9.48780938168963,-2.84862442585767,1.50713517738359));
#22188=CARTESIAN_POINT('Ctrl Pts',(9.48780938168963,-2.84862442585767,1.5071351773836));
#22189=CARTESIAN_POINT('Ctrl Pts',(9.53185899985944,-2.84862442585767,1.71160247880986));
#22190=CARTESIAN_POINT('Ctrl Pts',(9.58587318685495,-2.84862442792121,1.91525078718682));
#22191=CARTESIAN_POINT('Ctrl Pts',(9.70094960223702,-2.84862442792121,2.2980896617317));
#22192=CARTESIAN_POINT('Ctrl Pts',(9.76180678295297,-2.84862442585767,2.48053952383311));
#22193=CARTESIAN_POINT('Ctrl Pts',(9.8318097489011,-2.84862442585767,2.67629614457399));
#22194=CARTESIAN_POINT('Ctrl Pts',(9.83762325462799,-2.84862442585767,2.69245362484614));
#22195=CARTESIAN_POINT('Ctrl Pts',(9.84346698885961,-2.84862442585767,2.70859905909217));
#22196=CARTESIAN_POINT('',(9.24126248314343,-2.84862442585767,1.50713517738358));
#22197=CARTESIAN_POINT('',(13.3346225254169,-2.84862442585767,1.50713517738359));
#22198=CARTESIAN_POINT('',(8.77665942204888,-2.84682623267641,2.71029357829656));
#22199=CARTESIAN_POINT('Ctrl Pts',(8.77679361475528,-2.84862442585767,2.70860756651644));
#22200=CARTESIAN_POINT('Ctrl Pts',(8.78379792777184,-2.84862442585767,2.69251369706502));
#22201=CARTESIAN_POINT('Ctrl Pts',(8.79078230243175,-2.84862442585767,2.67640964375849));
#22202=CARTESIAN_POINT('Ctrl Pts',(8.8753576224118,-2.84862442585767,2.48069807460854));
#22203=CARTESIAN_POINT('Ctrl Pts',(8.95123295617157,-2.8486244273253,2.29789414186475));
#22204=CARTESIAN_POINT('Ctrl Pts',(9.10046525102538,-2.8486244273253,1.91583271764201));
#22205=CARTESIAN_POINT('Ctrl Pts',(9.17497777181831,-2.84862442585767,1.71136117817557));
#22206=CARTESIAN_POINT('Ctrl Pts',(9.24126248314343,-2.84862442585767,1.50713517738359));
#22207=CARTESIAN_POINT('',(8.59333237745357,-2.84682736201,2.71029427388594));
#22208=CARTESIAN_POINT('',(11.0238490761438,-2.84862442585767,2.71179421793157));
#22209=CARTESIAN_POINT('',(8.23780938168963,-2.84862442585767,1.50713517738359));
#22210=CARTESIAN_POINT('Ctrl Pts',(8.23780938168964,-2.84862442585767,1.5071351773836));
#22211=CARTESIAN_POINT('Ctrl Pts',(8.28185902228173,-2.84862442585767,1.7116025828885));
#22212=CARTESIAN_POINT('Ctrl Pts',(8.33587259560373,-2.84862442791195,1.91525079323359));
#22213=CARTESIAN_POINT('Ctrl Pts',(8.45094825529517,-2.84862442791195,2.29809205765932));
#22214=CARTESIAN_POINT('Ctrl Pts',(8.51180523038482,-2.84862442585767,2.48054376287594));
#22215=CARTESIAN_POINT('Ctrl Pts',(8.58180849741605,-2.84862442585767,2.67630369365445));
#22216=CARTESIAN_POINT('Ctrl Pts',(8.58762237980882,-2.84862442585767,2.69246241698621));
#22217=CARTESIAN_POINT('Ctrl Pts',(8.59346649505355,-2.84862442585767,2.70860909277272));
#22218=CARTESIAN_POINT('',(7.99126248314343,-2.84862442585767,1.50713517738358));
#22219=CARTESIAN_POINT('',(13.3346225254169,-2.84862442585767,1.50713517738359));
#22220=CARTESIAN_POINT('',(7.526659415135,-2.84683427137387,2.71029850822801));
#22221=CARTESIAN_POINT('Ctrl Pts',(7.52679307496196,-2.84862442585767,2.70861838061488));
#22222=CARTESIAN_POINT('Ctrl Pts',(7.53379789201695,-2.84862442585767,2.6925231903734));
#22223=CARTESIAN_POINT('Ctrl Pts',(7.54078276765018,-2.84862442585767,2.67641781492382));
#22224=CARTESIAN_POINT('Ctrl Pts',(7.62535873067299,-2.84862442585767,2.48070267374547));
#22225=CARTESIAN_POINT('Ctrl Pts',(7.70123402906389,-2.84862442731812,2.29789681034083));
#22226=CARTESIAN_POINT('Ctrl Pts',(7.85046588841197,-2.84862442731812,1.91583267628874));
#22227=CARTESIAN_POINT('Ctrl Pts',(7.92497771912674,-2.84862442585767,1.7113613405205));
#22228=CARTESIAN_POINT('Ctrl Pts',(7.99126248314342,-2.84862442585767,1.5071351773836));
#22229=CARTESIAN_POINT('',(7.34333236934253,-2.846835520603,2.71029927000383));
#22230=CARTESIAN_POINT('',(11.0238490761438,-2.84862442585767,2.71179421793157));
#22231=CARTESIAN_POINT('',(6.98780938168963,-2.84862442585767,1.50713517738359));
#22232=CARTESIAN_POINT('Ctrl Pts',(6.98780938168963,-2.84862442585767,1.5071351773836));
#22233=CARTESIAN_POINT('Ctrl Pts',(7.0318590477534,-2.84862442585767,1.71160270112162));
#22234=CARTESIAN_POINT('Ctrl Pts',(7.08587194364161,-2.84862442790181,1.91525079631235));
#22235=CARTESIAN_POINT('Ctrl Pts',(7.20094677397292,-2.84862442790181,2.29809467489166));
#22236=CARTESIAN_POINT('Ctrl Pts',(7.26180352074679,-2.84862442585766,2.48054838492829));
#22237=CARTESIAN_POINT('Ctrl Pts',(7.33180711870137,-2.84862442585766,2.67631193139019));
#22238=CARTESIAN_POINT('Ctrl Pts',(7.33762141389105,-2.84862442585767,2.69247201579432));
#22239=CARTESIAN_POINT('Ctrl Pts',(7.34346594671238,-2.84862442585767,2.70862005097966));
#22240=CARTESIAN_POINT('',(6.74126248314343,-2.84862442585767,1.50713517738358));
#22241=CARTESIAN_POINT('',(13.3346225254169,-2.84862442585767,1.50713517738359));
#22242=CARTESIAN_POINT('',(6.2766593992019,-2.84684318562975,2.71030391984611));
#22243=CARTESIAN_POINT('Ctrl Pts',(6.27679247260682,-2.84862442585767,2.70863024324506));
#22244=CARTESIAN_POINT('Ctrl Pts',(6.28379784512061,-2.84862442585767,2.69253359968691));
#22245=CARTESIAN_POINT('Ctrl Pts',(6.29078327281752,-2.84862442585768,2.67642676942568));
#22246=CARTESIAN_POINT('Ctrl Pts',(6.37535994854178,-2.84862442585768,2.48070770856496));
#22247=CARTESIAN_POINT('Ctrl Pts',(6.45123520736229,-2.84862442731026,2.29789973691976));
#22248=CARTESIAN_POINT('Ctrl Pts',(6.60046659256744,-2.84862442731026,1.91583262505285));
#22249=CARTESIAN_POINT('Ctrl Pts',(6.67497765942542,-2.84862442585767,1.71136152446282));
#22250=CARTESIAN_POINT('Ctrl Pts',(6.74126248314343,-2.84862442585767,1.50713517738359));
#22251=CARTESIAN_POINT('',(6.09333235190302,-2.8468445755701,2.71030475869925));
#22252=CARTESIAN_POINT('',(11.0238490761438,-2.84862442585767,2.71179421793157));
#22253=CARTESIAN_POINT('',(5.73780938168963,-2.84862442585767,1.50713517738359));
#22254=CARTESIAN_POINT('Ctrl Pts',(5.73780938168963,-2.84862442585767,1.5071351773836));
#22255=CARTESIAN_POINT('Ctrl Pts',(5.78185907685439,-2.84862442585767,1.71160283620116));
#22256=CARTESIAN_POINT('Ctrl Pts',(5.83587122068751,-2.84862442789063,1.91525079561866));
#22257=CARTESIAN_POINT('Ctrl Pts',(5.9509451358443,-2.84862442789063,2.29809754881907));
#22258=CARTESIAN_POINT('Ctrl Pts',(6.01180162763585,-2.84862442585767,2.48055345043311));
#22259=CARTESIAN_POINT('Ctrl Pts',(6.08180559131495,-2.84862442585767,2.67632096708642));
#22260=CARTESIAN_POINT('Ctrl Pts',(6.08762034133423,-2.84862442585767,2.69248254974333));
#22261=CARTESIAN_POINT('Ctrl Pts',(6.09346533427394,-2.84862442585767,2.70863208133986));
#22262=CARTESIAN_POINT('',(5.49126248314343,-2.84862442585767,1.50713517738358));
#22263=CARTESIAN_POINT('',(13.3346225254169,-2.84862442585767,1.50713517738359));
#22264=CARTESIAN_POINT('',(5.02665937189225,-2.84685313164047,2.71030989474673));
#22265=CARTESIAN_POINT('Ctrl Pts',(5.02679179614449,-2.84862442585767,2.70864333135427));
#22266=CARTESIAN_POINT('Ctrl Pts',(5.03379778445795,-2.84862442585767,2.69254507916332));
#22267=CARTESIAN_POINT('Ctrl Pts',(5.04078382417434,-2.84862442585766,2.67643663859843));
#22268=CARTESIAN_POINT('Ctrl Pts',(5.12536129472081,-2.84862442585766,2.48071325160255));
#22269=CARTESIAN_POINT('Ctrl Pts',(5.20123650898541,-2.84862442730161,2.29790296509866));
#22270=CARTESIAN_POINT('Ctrl Pts',(5.35046737523669,-2.84862442730161,1.91583256170217));
#22271=CARTESIAN_POINT('Ctrl Pts',(5.42497759134768,-2.84862442585767,1.7113617342132));
#22272=CARTESIAN_POINT('Ctrl Pts',(5.49126248314342,-2.84862442585767,1.5071351773836));
#22273=CARTESIAN_POINT('',(4.84333232268694,-2.84685468828742,2.71031082423224));
#22274=CARTESIAN_POINT('',(11.0238490761438,-2.84862442585767,2.71179421793157));
#22275=CARTESIAN_POINT('',(4.48780938168963,-2.84862442585767,1.50713517738359));
#22276=CARTESIAN_POINT('Ctrl Pts',(4.48780938168963,-2.84862442585767,1.5071351773836));
#22277=CARTESIAN_POINT('Ctrl Pts',(4.53185911031318,-2.84862442585767,1.71160299150844));
#22278=CARTESIAN_POINT('Ctrl Pts',(4.58587041394647,-2.84862442787828,1.9152507901144));
#22279=CARTESIAN_POINT('Ctrl Pts',(4.70094331303715,-2.84862442787828,2.29810072324551));
#22280=CARTESIAN_POINT('Ctrl Pts',(4.76179951821517,-2.84862442585766,2.48055903410995));
#22281=CARTESIAN_POINT('Ctrl Pts',(4.83180388858748,-2.84862442585766,2.67633093595801));
#22282=CARTESIAN_POINT('Ctrl Pts',(4.83761914279346,-2.84862442585767,2.69249417782208));
#22283=CARTESIAN_POINT('Ctrl Pts',(4.84346464580177,-2.84862442585767,2.70864536656847));
#22284=CARTESIAN_POINT('',(4.24126248314343,-2.84862442585767,1.50713517738358));
#22285=CARTESIAN_POINT('',(13.3346225254169,-2.84862442585767,1.50713517738359));
#22286=CARTESIAN_POINT('',(3.77665933013941,-2.84686430560633,2.71031653510881));
#22287=CARTESIAN_POINT('Ctrl Pts',(3.77679103100252,-2.84862442585767,2.70865786644558));
#22288=CARTESIAN_POINT('Ctrl Pts',(3.78379770666065,-2.84862442585767,2.69255782170753));
#22289=CARTESIAN_POINT('Ctrl Pts',(3.7907844294769,-2.84862442585767,2.6764475867298));
#22290=CARTESIAN_POINT('Ctrl Pts',(3.87536279264918,-2.84862442585767,2.48071939353203));
#22291=CARTESIAN_POINT('Ctrl Pts',(3.95123795638205,-2.84862442729201,2.29790654931287));
#22292=CARTESIAN_POINT('Ctrl Pts',(4.10046825118152,-2.84862442729201,1.91583248336832));
#22293=CARTESIAN_POINT('Ctrl Pts',(4.17497751316149,-2.84862442585767,1.71136197510816));
#22294=CARTESIAN_POINT('Ctrl Pts',(4.24126248314342,-2.84862442585767,1.5071351773836));
#22295=CARTESIAN_POINT('',(3.5933397832319,-2.84842713334438,2.71177821818276));
#22296=CARTESIAN_POINT('',(11.0238490761438,-2.84862442585767,2.71179421793157));
#22297=CARTESIAN_POINT('',(3.23780938168963,-2.84862442585767,1.50713517738359));
#22298=CARTESIAN_POINT('Ctrl Pts',(3.23780938168963,-2.84862442585767,1.50713517738361));
#22299=CARTESIAN_POINT('Ctrl Pts',(3.28186054745108,-2.84862442585767,1.71160966234283));
#22300=CARTESIAN_POINT('Ctrl Pts',(3.33582269739854,-2.84862442724084,1.91524933773065));
#22301=CARTESIAN_POINT('Ctrl Pts',(3.45073483075678,-2.84862442724084,2.2979205346272));
#22302=CARTESIAN_POINT('Ctrl Pts',(3.51144589960124,-2.84862442585768,2.48014616288996));
#22303=CARTESIAN_POINT('Ctrl Pts',(3.58146712224872,-2.84862442585768,2.67616260726964));
#22304=CARTESIAN_POINT('Ctrl Pts',(3.58743530933706,-2.84862442585767,2.69276463740784));
#22305=CARTESIAN_POINT('Ctrl Pts',(3.59343543922426,-2.84862442585767,2.70935393890616));
#22306=CARTESIAN_POINT('',(3.02384907614375,-2.84862442585767,1.50713517738359));
#22307=CARTESIAN_POINT('',(13.3346225254169,-2.84862442585767,1.50713517738359));
#22308=CARTESIAN_POINT('',(3.02365448843556,-2.84819869582995,-2.12611758856074));
#22309=CARTESIAN_POINT('',(3.02384907614375,-2.84862442585767,-1.40404227860195));
#22310=CARTESIAN_POINT('',(3.18488877059788,-2.84862442585766,-1.50713517738361));
#22311=CARTESIAN_POINT('Ctrl Pts',(3.18488877059788,-2.84862442585767,-1.50713517738361));
#22312=CARTESIAN_POINT('Ctrl Pts',(3.16242044753531,-2.84862442585767,-1.61142750896447));
#22313=CARTESIAN_POINT('Ctrl Pts',(3.137405991007,-2.84862442595863,-1.71531300796113));
#22314=CARTESIAN_POINT('Ctrl Pts',(3.0834656597595,-2.84862442595863,-1.92105514468293));
#22315=CARTESIAN_POINT('Ctrl Pts',(3.0544704326137,-2.84862442585767,-2.02327555320667));
#22316=CARTESIAN_POINT('Ctrl Pts',(3.02384907614375,-2.84862442585767,-2.12477398354848));
#22317=CARTESIAN_POINT('',(3.43143566914408,-2.84862442585766,-1.5071351773836));
#22318=CARTESIAN_POINT('',(13.3346225254169,-2.84862442585767,-1.50713517738359));
#22319=CARTESIAN_POINT('',(3.89603880551603,-2.84686020278407,-2.71031410533045));
#22320=CARTESIAN_POINT('Ctrl Pts',(3.89590683973102,-2.84862442585767,-2.70865254916596));
#22321=CARTESIAN_POINT('Ctrl Pts',(3.88889722083,-2.84862442585767,-2.69254581918906));
#22322=CARTESIAN_POINT('Ctrl Pts',(3.88190757115915,-2.84862442585768,-2.67642888977708));
#22323=CARTESIAN_POINT('Ctrl Pts',(3.79732623229834,-2.84862442585768,-2.48069416593426));
#22324=CARTESIAN_POINT('Ctrl Pts',(3.7214509531498,-2.84862442738219,-2.29788126150319));
#22325=CARTESIAN_POINT('Ctrl Pts',(3.57222405172544,-2.84862442738219,-1.91581557178352));
#22326=CARTESIAN_POINT('Ctrl Pts',(3.49771788311829,-2.84862442585767,-1.71135348373173));
#22327=CARTESIAN_POINT('Ctrl Pts',(3.43143566914408,-2.84862442585767,-1.50713517738359));
#22328=CARTESIAN_POINT('',(4.07936584331022,-2.84685855096328,-2.71031312437899));
#22329=CARTESIAN_POINT('',(11.0238490761438,-2.84862442585767,-2.71179421793157));
#22330=CARTESIAN_POINT('',(4.43488877059788,-2.84862442585766,-1.50713517738361));
#22331=CARTESIAN_POINT('Ctrl Pts',(4.43488877059788,-2.84862442585767,-1.50713517738361));
#22332=CARTESIAN_POINT('Ctrl Pts',(4.39082934716643,-2.84862442585767,-1.71164799237998));
#22333=CARTESIAN_POINT('Ctrl Pts',(4.33680421314192,-2.84862442782486,-1.91534068114032));
#22334=CARTESIAN_POINT('Ctrl Pts',(4.22171428517076,-2.84862442782486,-2.29822947317743));
#22335=CARTESIAN_POINT('Ctrl Pts',(4.16085761026589,-2.84862442585767,-2.48068346557449));
#22336=CARTESIAN_POINT('Ctrl Pts',(4.09086679229697,-2.84862442585767,-2.67641287300669));
#22337=CARTESIAN_POINT('Ctrl Pts',(4.08506533437374,-2.84862442585767,-2.69253763418667));
#22338=CARTESIAN_POINT('Ctrl Pts',(4.07923377064371,-2.84862442585767,-2.70865040206242));
#22339=CARTESIAN_POINT('',(4.68143566914408,-2.84862442585766,-1.5071351773836));
#22340=CARTESIAN_POINT('',(13.3346225254169,-2.84862442585767,-1.50713517738359));
#22341=CARTESIAN_POINT('',(5.14603876927131,-2.8468494881385,-2.71030771333065));
#22342=CARTESIAN_POINT('Ctrl Pts',(5.14590610781719,-2.84862442585767,-2.70863855402169));
#22343=CARTESIAN_POINT('Ctrl Pts',(5.13889714963154,-2.84862442585767,-2.69253354823215));
#22344=CARTESIAN_POINT('Ctrl Pts',(5.13190815660042,-2.84862442585766,-2.67641834479668));
#22345=CARTESIAN_POINT('Ctrl Pts',(5.04732767386717,-2.84862442585766,-2.48068824836471));
#22346=CARTESIAN_POINT('Ctrl Pts',(4.97145234642707,-2.8486244273917,-2.29787781119133));
#22347=CARTESIAN_POINT('Ctrl Pts',(4.82222489298551,-2.8486244273917,-1.91581564514287));
#22348=CARTESIAN_POINT('Ctrl Pts',(4.74771780885373,-2.84862442585767,-1.71135325491949));
#22349=CARTESIAN_POINT('Ctrl Pts',(4.68143566914408,-2.84862442585767,-1.50713517738359));
#22350=CARTESIAN_POINT('',(5.3293658092159,-2.84684801847815,-2.71030683105326));
#22351=CARTESIAN_POINT('',(11.0238490761438,-2.84862442585767,-2.71179421793157));
#22352=CARTESIAN_POINT('',(5.68488877059788,-2.84862442585766,-1.50713517738361));
#22353=CARTESIAN_POINT('Ctrl Pts',(5.68488877059787,-2.84862442585767,-1.50713517738361));
#22354=CARTESIAN_POINT('Ctrl Pts',(5.64082938247698,-2.84862442585767,-1.71164782847729));
#22355=CARTESIAN_POINT('Ctrl Pts',(5.58680337295899,-2.84862442783755,-1.91534068797091));
#22356=CARTESIAN_POINT('Ctrl Pts',(5.47171238880716,-2.84862442783755,-2.29822617883969));
#22357=CARTESIAN_POINT('Ctrl Pts',(5.41085541472201,-2.84862442585768,-2.48067767630624));
#22358=CARTESIAN_POINT('Ctrl Pts',(5.34086501982091,-2.84862442585768,-2.67640253517119));
#22359=CARTESIAN_POINT('Ctrl Pts',(5.335064085706,-2.84862442585767,-2.69252557390748));
#22360=CARTESIAN_POINT('Ctrl Pts',(5.32923305188914,-2.84862442585767,-2.70863662146847));
#22361=CARTESIAN_POINT('',(5.93143566914408,-2.84862442585766,-1.5071351773836));
#22362=CARTESIAN_POINT('',(13.3346225254169,-2.84862442585767,-1.50713517738359));
#22363=CARTESIAN_POINT('',(6.3960387462905,-2.84683992679533,-2.71030194794593));
#22364=CARTESIAN_POINT('Ctrl Pts',(6.39590545902977,-2.84862442585767,-2.70862592165797));
#22365=CARTESIAN_POINT('Ctrl Pts',(6.38889709426525,-2.84862442585767,-2.69252246698333));
#22366=CARTESIAN_POINT('Ctrl Pts',(6.381908691017,-2.84862442585767,-2.67640881627049));
#22367=CARTESIAN_POINT('Ctrl Pts',(6.29732897257062,-2.84862442585767,-2.48068289513417));
#22368=CARTESIAN_POINT('Ctrl Pts',(6.22145360243729,-2.8486244274003,-2.29787469612044));
#22369=CARTESIAN_POINT('Ctrl Pts',(6.07222564657022,-2.8486244274003,-1.91581570455012));
#22370=CARTESIAN_POINT('Ctrl Pts',(5.99771774402429,-2.84862442585767,-1.71135305517723));
#22371=CARTESIAN_POINT('Ctrl Pts',(5.93143566914408,-2.84862442585767,-1.50713517738359));
#22372=CARTESIAN_POINT('',(6.57936578792838,-2.84683861010252,-2.71030114914197));
#22373=CARTESIAN_POINT('',(11.0238490761438,-2.84862442585767,-2.71179421793157));
#22374=CARTESIAN_POINT('',(6.93488877059788,-2.84862442585766,-1.50713517738361));
#22375=CARTESIAN_POINT('Ctrl Pts',(6.93488877059789,-2.84862442585767,-1.5071351773836));
#22376=CARTESIAN_POINT('Ctrl Pts',(6.89082941311706,-2.84862442585767,-1.71164768625373));
#22377=CARTESIAN_POINT('Ctrl Pts',(6.83680262185114,-2.84862442784899,-1.91534068961923));
#22378=CARTESIAN_POINT('Ctrl Pts',(6.72171068862222,-2.84862442784899,-2.29822320309697));
#22379=CARTESIAN_POINT('Ctrl Pts',(6.66085344903225,-2.84862442585767,-2.48067243596248));
#22380=CARTESIAN_POINT('Ctrl Pts',(6.59086343368136,-2.84862442585767,-2.67639318603298));
#22381=CARTESIAN_POINT('Ctrl Pts',(6.58506297100052,-2.84862442585767,-2.69251467300301));
#22382=CARTESIAN_POINT('Ctrl Pts',(6.5792324140922,-2.84862442585767,-2.70862417070381));
#22383=CARTESIAN_POINT('',(7.18143566914408,-2.84862442585767,-1.5071351773836));
#22384=CARTESIAN_POINT('',(13.3346225254169,-2.84862442585767,-1.50713517738359));
#22385=CARTESIAN_POINT('',(7.64603873378328,-2.84683133801731,-2.71029671495572));
#22386=CARTESIAN_POINT('Ctrl Pts',(7.64590487996825,-2.84862442585767,-2.70861444779753));
#22387=CARTESIAN_POINT('Ctrl Pts',(7.63889705165458,-2.84862442585767,-2.69251239752542));
#22388=CARTESIAN_POINT('Ctrl Pts',(7.63190918158326,-2.84862442585767,-2.67640015265958));
#22389=CARTESIAN_POINT('Ctrl Pts',(7.54733015001958,-2.84862442585767,-2.48067802259182));
#22390=CARTESIAN_POINT('Ctrl Pts',(7.47145474188106,-2.84862442740813,-2.29787186609686));
#22391=CARTESIAN_POINT('Ctrl Pts',(7.3222263260763,-2.84862442740813,-1.91581575263515));
#22392=CARTESIAN_POINT('Ctrl Pts',(7.2477176870411,-2.84862442585767,-1.7113528796096));
#22393=CARTESIAN_POINT('Ctrl Pts',(7.18143566914408,-2.84862442585767,-1.50713517738359));
#22394=CARTESIAN_POINT('',(7.82936577676323,-2.84683015106684,-2.71029598749509));
#22395=CARTESIAN_POINT('',(11.0238490761438,-2.84862442585767,-2.71179421793157));
#22396=CARTESIAN_POINT('',(8.18488877059788,-2.84862442585766,-1.50713517738361));
#22397=CARTESIAN_POINT('Ctrl Pts',(8.18488877059787,-2.84862442585767,-1.50713517738361));
#22398=CARTESIAN_POINT('Ctrl Pts',(8.14082943988044,-2.84862442585767,-1.71164756202476));
#22399=CARTESIAN_POINT('Ctrl Pts',(8.08680194594983,-2.84862442785935,-1.91534068721287));
#22400=CARTESIAN_POINT('Ctrl Pts',(7.97170915442048,-2.84862442785935,-2.29822049854839));
#22401=CARTESIAN_POINT('Ctrl Pts',(7.910851677616,-2.84862442585767,-2.48066766373789));
#22402=CARTESIAN_POINT('Ctrl Pts',(7.84086200497834,-2.84862442585767,-2.67638467936083));
#22403=CARTESIAN_POINT('Ctrl Pts',(7.83506196928568,-2.84862442585767,-2.69250475952157));
#22404=CARTESIAN_POINT('Ctrl Pts',(7.82923184430401,-2.84862442585767,-2.70861285213785));
#22405=CARTESIAN_POINT('',(8.43143566914408,-2.84862442585767,-1.5071351773836));
#22406=CARTESIAN_POINT('',(13.3346225254169,-2.84862442585767,-1.50713517738359));
#22407=CARTESIAN_POINT('',(8.89603872959521,-2.84682357725585,-2.71029193875473));
#22408=CARTESIAN_POINT('Ctrl Pts',(8.89590435996554,-2.84862442585767,-2.70860396846321));
#22409=CARTESIAN_POINT('Ctrl Pts',(8.88889701939368,-2.84862442585767,-2.69250319699323));
#22410=CARTESIAN_POINT('Ctrl Pts',(8.881909634102,-2.84862442585767,-2.67639223223817));
#22411=CARTESIAN_POINT('Ctrl Pts',(8.79733122354344,-2.84862442585767,-2.48067356350021));
#22412=CARTESIAN_POINT('Ctrl Pts',(8.72145578136366,-2.84862442741529,-2.29786928082383));
#22413=CARTESIAN_POINT('Ctrl Pts',(8.57222694237506,-2.84862442741529,-1.91581579145778));
#22414=CARTESIAN_POINT('Ctrl Pts',(8.49771763664538,-2.84862442585767,-1.71135272433826));
#22415=CARTESIAN_POINT('Ctrl Pts',(8.43143566914408,-2.84862442585767,-1.50713517738359));
#22416=CARTESIAN_POINT('',(9.07936577364419,-2.84682250133587,-2.71029127282857));
#22417=CARTESIAN_POINT('',(11.0238490761438,-2.84862442585767,-2.71179421793157));
#22418=CARTESIAN_POINT('',(9.43488877059788,-2.84862442585766,-1.5071351773836));
#22419=CARTESIAN_POINT('Ctrl Pts',(9.43488877059788,-2.84862442585767,-1.50713517738359));
#22420=CARTESIAN_POINT('Ctrl Pts',(9.39082946339622,-2.84862442585767,-1.71164745287044));
#22421=CARTESIAN_POINT('Ctrl Pts',(9.33680133416077,-2.8486244278688,-1.91534068162397));
#22422=CARTESIAN_POINT('Ctrl Pts',(9.2217077620153,-2.8486244278688,-2.29821802707406));
#22423=CARTESIAN_POINT('Ctrl Pts',(9.16085007199191,-2.84862442585767,-2.48066329456691));
#22424=CARTESIAN_POINT('Ctrl Pts',(9.09086071058218,-2.84862442585767,-2.67637689747843));
#22425=CARTESIAN_POINT('Ctrl Pts',(9.08506106379369,-2.84862442585767,-2.69249569513711));
#22426=CARTESIAN_POINT('Ctrl Pts',(9.07923133219744,-2.84862442585767,-2.70860250681946));
#22427=CARTESIAN_POINT('',(9.68143566914408,-2.84862442585767,-1.5071351773836));
#22428=CARTESIAN_POINT('',(13.3346225254169,-2.84862442585767,-1.50713517738359));
#22429=CARTESIAN_POINT('',(10.1460387320439,-2.84681652750098,-2.71028755790189));
#22430=CARTESIAN_POINT('Ctrl Pts',(10.1459038904249,-2.84862442585767,-2.70859435034995));
#22431=CARTESIAN_POINT('Ctrl Pts',(10.1388969955833,-2.84862442585767,-2.69249474921214));
#22432=CARTESIAN_POINT('Ctrl Pts',(10.1319100533288,-2.84862442585767,-2.67638495598403));
#22433=CARTESIAN_POINT('Ctrl Pts',(10.0473322072149,-2.84862442585767,-2.48066946312399));
#22434=CARTESIAN_POINT('Ctrl Pts',(9.97145673437474,-2.84862442742187,-2.29786690753779));
#22435=CARTESIAN_POINT('Ctrl Pts',(9.82222750426836,-2.84862442742187,-1.91581582264984));
#22436=CARTESIAN_POINT('Ctrl Pts',(9.74771759182774,-2.84862442585767,-1.71135258625323));
#22437=CARTESIAN_POINT('Ctrl Pts',(9.68143566914409,-2.84862442585767,-1.50713517738361));
#22438=CARTESIAN_POINT('',(10.3293573795468,-2.84839556406923,-2.71178786142128));
#22439=CARTESIAN_POINT('',(11.0238490761438,-2.84862442585767,-2.71179421793157));
#22440=CARTESIAN_POINT('',(10.6848887705979,-2.84862442585766,-1.5071351773836));
#22441=CARTESIAN_POINT('Ctrl Pts',(10.6848887705979,-2.84862442585767,-1.50713517738359));
#22442=CARTESIAN_POINT('Ctrl Pts',(10.6408288271577,-2.84862442585767,-1.71165040613047));
#22443=CARTESIAN_POINT('Ctrl Pts',(10.586823565171,-2.84862442755607,-1.9153402145107));
#22444=CARTESIAN_POINT('Ctrl Pts',(10.4718028413942,-2.84862442755607,-2.29814280868909));
#22445=CARTESIAN_POINT('Ctrl Pts',(10.4110099703332,-2.84862442585767,-2.48048848453579));
#22446=CARTESIAN_POINT('Ctrl Pts',(10.3410124389629,-2.84862442585767,-2.67631715615895));
#22447=CARTESIAN_POINT('Ctrl Pts',(10.3351441403831,-2.84862442585767,-2.69263311564845));
#22448=CARTESIAN_POINT('Ctrl Pts',(10.3292450042586,-2.84862442585767,-2.70893678933792));
#22449=CARTESIAN_POINT('',(13.3346225254169,-2.84862442585767,-1.50713517738359));
#22450=CARTESIAN_POINT('Origin',(3.02384907614375,2.84862442585767,2.80808455720391));
#22451=CARTESIAN_POINT('',(10.6516571958764,2.84853760141617,-2.71188542038896));
#22452=CARTESIAN_POINT('',(11.0238490761438,2.84862442585767,-1.77841863815956));
#22453=CARTESIAN_POINT('Ctrl Pts',(10.6517444165533,2.84862442585767,-2.70958663119422));
#22454=CARTESIAN_POINT('Ctrl Pts',(10.7181155081048,2.84862442585767,-2.5572180519126));
#22455=CARTESIAN_POINT('Ctrl Pts',(10.7831857927431,2.84862442636543,-2.40277143381646));
#22456=CARTESIAN_POINT('Ctrl Pts',(10.9075012055968,2.84862442636543,-2.09344139364087));
#22457=CARTESIAN_POINT('Ctrl Pts',(10.9677673094432,2.84862442585767,-1.93595017012862));
#22458=CARTESIAN_POINT('Ctrl Pts',(11.0238490761437,2.84862442585767,-1.77841863815954));
#22459=CARTESIAN_POINT('',(10.4683323761737,2.84681652750097,-2.71028755790189));
#22460=CARTESIAN_POINT('',(11.0238490761438,2.84862442585767,-2.71179421793157));
#22461=CARTESIAN_POINT('',(10.1128093816896,2.84862442585767,-1.50713517738358));
#22462=CARTESIAN_POINT('Ctrl Pts',(10.1128093816896,2.84862442585767,-1.50713517738361));
#22463=CARTESIAN_POINT('Ctrl Pts',(10.1568589896422,2.84862442585767,-1.71160243138402));
#22464=CARTESIAN_POINT('Ctrl Pts',(10.2108734623886,2.84862442792555,-1.91525078325235));
#22465=CARTESIAN_POINT('Ctrl Pts',(10.3259502311565,2.84862442792555,-2.29808853750365));
#22466=CARTESIAN_POINT('Ctrl Pts',(10.3868075072088,2.84862442585767,-2.48053753211887));
#22467=CARTESIAN_POINT('Ctrl Pts',(10.4568103325124,2.84862442585767,-2.6762925996824));
#22468=CARTESIAN_POINT('Ctrl Pts',(10.4626236619148,2.84862442585767,-2.69244949767383));
#22469=CARTESIAN_POINT('Ctrl Pts',(10.4684672177927,2.84862442585767,-2.70859435034994));
#22470=CARTESIAN_POINT('',(9.86626248314343,2.84862442585767,-1.50713517738359));
#22471=CARTESIAN_POINT('',(13.3346225254169,2.84862442585767,-1.50713517738359));
#22472=CARTESIAN_POINT('',(9.40165942271325,2.8468225013359,-2.71029127282857));
#22473=CARTESIAN_POINT('Ctrl Pts',(9.40179386416001,2.84862442585767,-2.70860250681946));
#22474=CARTESIAN_POINT('Ctrl Pts',(9.40879794213361,2.84862442585767,-2.69250925396209));
#22475=CARTESIAN_POINT('Ctrl Pts',(9.41578208317429,2.84862442585767,-2.67640581787988));
#22476=CARTESIAN_POINT('Ctrl Pts',(9.50035710454219,2.84862442585767,-2.48069591960582));
#22477=CARTESIAN_POINT('Ctrl Pts',(9.57623245461227,2.84862442732866,-2.29789289314525));
#22478=CARTESIAN_POINT('Ctrl Pts',(9.72546495433774,2.84862442732866,-1.91583273517924));
#22479=CARTESIAN_POINT('Ctrl Pts',(9.79997779588513,2.84862442585767,-1.71136110402466));
#22480=CARTESIAN_POINT('Ctrl Pts',(9.86626248314343,2.84862442585767,-1.50713517738359));
#22481=CARTESIAN_POINT('',(9.21833237862236,2.84682357725585,-2.71029193875473));
#22482=CARTESIAN_POINT('',(11.0238490761438,2.84862442585767,-2.71179421793157));
#22483=CARTESIAN_POINT('',(8.86280938168963,2.84862442585767,-1.50713517738358));
#22484=CARTESIAN_POINT('Ctrl Pts',(8.86280938168963,2.84862442585767,-1.5071351773836));
#22485=CARTESIAN_POINT('Ctrl Pts',(8.90685901072075,2.84862442585767,-1.71160252922533));
#22486=CARTESIAN_POINT('Ctrl Pts',(8.96087289825601,2.84862442791668,-1.91525079053687));
#22487=CARTESIAN_POINT('Ctrl Pts',(9.07594894433648,2.84862442791668,-2.29809083397137));
#22488=CARTESIAN_POINT('Ctrl Pts',(9.13680602485858,2.84862442585767,-2.48054159879405));
#22489=CARTESIAN_POINT('Ctrl Pts',(9.20680913788998,2.84862442585767,-2.67629983902876));
#22490=CARTESIAN_POINT('Ctrl Pts',(9.21262282775703,2.84862442585767,-2.69245792713028));
#22491=CARTESIAN_POINT('Ctrl Pts',(9.21846674825203,2.84862442585767,-2.70860396846321));
#22492=CARTESIAN_POINT('',(8.61626248314343,2.84862442585767,-1.50713517738359));
#22493=CARTESIAN_POINT('',(13.3346225254169,2.84862442585767,-1.50713517738359));
#22494=CARTESIAN_POINT('',(8.15165941959421,2.84683015106688,-2.71029598749509));
#22495=CARTESIAN_POINT('Ctrl Pts',(8.15179335205343,2.84862442585767,-2.70861285213785));
#22496=CARTESIAN_POINT('Ctrl Pts',(8.15879791114812,2.84862442585767,-2.69251833761412));
#22497=CARTESIAN_POINT('Ctrl Pts',(8.16578253039036,2.84862442585767,-2.67641363857816));
#22498=CARTESIAN_POINT('Ctrl Pts',(8.25035816386072,2.84862442585767,-2.48070032366843));
#22499=CARTESIAN_POINT('Ctrl Pts',(8.32623348041883,2.84862442732179,-2.29789544620645));
#22500=CARTESIAN_POINT('Ctrl Pts',(8.47546556201146,2.84862442732179,-1.91583269807888));
#22501=CARTESIAN_POINT('Ctrl Pts',(8.54997774627531,2.84862442585767,-1.71136125687463));
#22502=CARTESIAN_POINT('Ctrl Pts',(8.61626248314343,2.84862442585767,-1.50713517738358));
#22503=CARTESIAN_POINT('',(7.9683323744343,2.84683133801736,-2.71029671495571));
#22504=CARTESIAN_POINT('',(11.0238490761438,2.84862442585767,-2.71179421793157));
#22505=CARTESIAN_POINT('',(7.61280938168963,2.84862442585767,-1.50713517738358));
#22506=CARTESIAN_POINT('Ctrl Pts',(7.61280938168963,2.84862442585767,-1.5071351773836));
#22507=CARTESIAN_POINT('Ctrl Pts',(7.65685903460308,2.84862442585767,-1.71160264008112));
#22508=CARTESIAN_POINT('Ctrl Pts',(7.71087227780285,2.84862442790699,-1.91525079518883));
#22509=CARTESIAN_POINT('Ctrl Pts',(7.82594753272231,2.84862442790699,-2.29809333657086));
#22510=CARTESIAN_POINT('Ctrl Pts',(7.88680439671883,2.84862442585767,-2.48054602253814));
#22511=CARTESIAN_POINT('Ctrl Pts',(7.9568078251961,2.84862442585767,-2.67630772013523));
#22512=CARTESIAN_POINT('Ctrl Pts',(7.96262190913101,2.84862442585767,-2.69246710814726));
#22513=CARTESIAN_POINT('Ctrl Pts',(7.96846622824932,2.84862442585767,-2.70861444779752));
#22514=CARTESIAN_POINT('',(7.36626248314343,2.84862442585767,-1.50713517738359));
#22515=CARTESIAN_POINT('',(13.3346225254169,2.84862442585767,-1.50713517738359));
#22516=CARTESIAN_POINT('',(6.90165940842906,2.84683861010255,-2.71030114914197));
#22517=CARTESIAN_POINT('Ctrl Pts',(6.90179278226525,2.84862442585767,-2.70862417070381));
#22518=CARTESIAN_POINT('Ctrl Pts',(6.90879787011014,2.84862442585767,-2.69252827167807));
#22519=CARTESIAN_POINT('Ctrl Pts',(6.91578301488098,2.84862442585767,-2.67642218671447));
#22520=CARTESIAN_POINT('Ctrl Pts',(7.00035932483387,2.84862442585767,-2.48070513252597));
#22521=CARTESIAN_POINT('Ctrl Pts',(7.07623460400956,2.84862442731428,-2.29789823886797));
#22522=CARTESIAN_POINT('Ctrl Pts',(7.2254662314708,2.84862442731428,-1.91583265203173));
#22523=CARTESIAN_POINT('Ctrl Pts',(7.29997769023056,2.84862442585767,-1.71136142955089));
#22524=CARTESIAN_POINT('Ctrl Pts',(7.36626248314343,2.84862442585767,-1.50713517738359));
#22525=CARTESIAN_POINT('',(6.71833236192707,2.84683992679534,-2.71030194794594));
#22526=CARTESIAN_POINT('',(11.0238490761438,2.84862442585767,-2.71179421793157));
#22527=CARTESIAN_POINT('',(6.36280938168963,2.84862442585767,-1.50713517738358));
#22528=CARTESIAN_POINT('Ctrl Pts',(6.36280938168963,2.84862442585767,-1.50713517738361));
#22529=CARTESIAN_POINT('Ctrl Pts',(6.40685906180869,2.84862442585767,-1.71160276636274));
#22530=CARTESIAN_POINT('Ctrl Pts',(6.46087159177102,2.84862442789636,-1.91525079649567));
#22531=CARTESIAN_POINT('Ctrl Pts',(6.57594597610578,2.84862442789636,-2.29809607725535));
#22532=CARTESIAN_POINT('Ctrl Pts',(6.63680259900565,2.84862442585767,-2.48055085796017));
#22533=CARTESIAN_POINT('Ctrl Pts',(6.70680637511918,2.84862442585767,-2.67631634173415));
#22534=CARTESIAN_POINT('Ctrl Pts',(6.71262089204982,2.84862442585767,-2.69247715675436));
#22535=CARTESIAN_POINT('Ctrl Pts',(6.7184656491878,2.84862442585767,-2.70862592165798));
#22536=CARTESIAN_POINT('',(6.11626248314343,2.84862442585767,-1.50713517738359));
#22537=CARTESIAN_POINT('',(13.3346225254169,2.84862442585767,-1.50713517738359));
#22538=CARTESIAN_POINT('',(5.65165938714153,2.84684801847819,-2.71030683105326));
#22539=CARTESIAN_POINT('Ctrl Pts',(5.6517921444683,2.84862442585767,-2.70863662146848));
#22540=CARTESIAN_POINT('Ctrl Pts',(5.65879781670129,2.84862442585767,-2.69253919463776));
#22541=CARTESIAN_POINT('Ctrl Pts',(5.66578354227913,2.84862442585766,-2.67643158029353));
#22542=CARTESIAN_POINT('Ctrl Pts',(5.75036060425611,2.84862442585766,-2.48071041137392));
#22543=CARTESIAN_POINT('Ctrl Pts',(5.82623584147821,2.84862442730604,-2.29790131019802));
#22544=CARTESIAN_POINT('Ctrl Pts',(5.97546697324722,2.84862442730604,-1.91583259505172));
#22545=CARTESIAN_POINT('Ctrl Pts',(6.04997762653236,2.84862442585767,-1.71136162580774));
#22546=CARTESIAN_POINT('Ctrl Pts',(6.11626248314343,2.84862442585767,-1.50713517738359));
#22547=CARTESIAN_POINT('',(5.46833233894627,2.84684948813853,-2.71030771333066));
#22548=CARTESIAN_POINT('',(11.0238490761438,2.84862442585767,-2.71179421793157));
#22549=CARTESIAN_POINT('',(5.11280938168963,2.84862442585767,-1.50713517738358));
#22550=CARTESIAN_POINT('Ctrl Pts',(5.11280938168963,2.84862442585767,-1.50713517738362));
#22551=CARTESIAN_POINT('Ctrl Pts',(5.15685909298675,2.84862442585767,-1.7116029110835));
#22552=CARTESIAN_POINT('Ctrl Pts',(5.2108708287094,2.84862442788461,-1.91525079354619));
#22553=CARTESIAN_POINT('Ctrl Pts',(5.3259442495258,2.84862442788461,-2.2980990953389));
#22554=CARTESIAN_POINT('Ctrl Pts',(5.38680060232149,2.84862442585766,-2.48055617216051));
#22555=CARTESIAN_POINT('Ctrl Pts',(5.45680476378349,2.84862442585766,-2.67632582520572));
#22556=CARTESIAN_POINT('Ctrl Pts',(5.46261975920138,2.84862442585767,-2.69248821564317));
#22557=CARTESIAN_POINT('Ctrl Pts',(5.46846500040038,2.84862442585767,-2.70863855402171));
#22558=CARTESIAN_POINT('',(4.86626248314343,2.84862442585767,-1.50713517738359));
#22559=CARTESIAN_POINT('',(13.3346225254169,2.84862442585767,-1.50713517738359));
#22560=CARTESIAN_POINT('',(4.40165935304722,2.84685855096331,-2.71031312437897));
#22561=CARTESIAN_POINT('Ctrl Pts',(4.40179142571374,2.84862442585767,-2.7086504020624));
#22562=CARTESIAN_POINT('Ctrl Pts',(4.40879774794817,2.84862442585767,-2.69255127864938));
#22563=CARTESIAN_POINT('Ctrl Pts',(4.41578411952675,2.84862442585767,-2.67644196595571));
#22564=CARTESIAN_POINT('Ctrl Pts',(4.50036202302706,2.84862442585767,-2.48071624117288));
#22565=CARTESIAN_POINT('Ctrl Pts',(4.5762372128446,2.84862442729694,-2.29790470877537));
#22566=CARTESIAN_POINT('Ctrl Pts',(4.72546780048414,2.84862442729694,-1.91583252461549));
#22567=CARTESIAN_POINT('Ctrl Pts',(4.79997755364427,2.84862442585767,-1.71136185037904));
#22568=CARTESIAN_POINT('Ctrl Pts',(4.86626248314343,2.84862442585767,-1.50713517738359));
#22569=CARTESIAN_POINT('',(4.21833230270155,2.8468602027841,-2.71031410533046));
#22570=CARTESIAN_POINT('',(11.0238490761438,2.84862442585767,-2.71179421793157));
#22571=CARTESIAN_POINT('',(3.86280938168963,2.84862442585767,-1.50713517738358));
#22572=CARTESIAN_POINT('Ctrl Pts',(3.86280938168963,2.84862442585767,-1.50713517738361));
#22573=CARTESIAN_POINT('Ctrl Pts',(3.90685912895696,2.84862442585767,-1.71160307804822));
#22574=CARTESIAN_POINT('Ctrl Pts',(3.9608699742735,2.84862442787157,-1.91525078515163));
#22575=CARTESIAN_POINT('Ctrl Pts',(4.07594232175518,2.84862442787157,-2.29810243978791));
#22576=CARTESIAN_POINT('Ctrl Pts',(4.13679836986563,2.84862442585768,-2.48056204862024));
#22577=CARTESIAN_POINT('Ctrl Pts',(4.20680296129537,2.84862442585768,-2.67633632166697));
#22578=CARTESIAN_POINT('Ctrl Pts',(4.21261848888836,2.84862442585767,-2.69250046252893));
#22579=CARTESIAN_POINT('Ctrl Pts',(4.21846426848655,2.84862442585767,-2.70865254916597));
#22580=CARTESIAN_POINT('',(3.61626248314343,2.84862442585767,-1.50713517738359));
#22581=CARTESIAN_POINT('',(13.3346225254169,2.84862442585767,-1.50713517738359));
#22582=CARTESIAN_POINT('',(3.15165930263079,2.84687042859227,-2.71032014408668));
#22583=CARTESIAN_POINT('Ctrl Pts',(3.15179060954266,2.84862442585767,-2.70866576166606));
#22584=CARTESIAN_POINT('Ctrl Pts',(3.15879766001169,2.84862442585767,-2.69256474069428));
#22585=CARTESIAN_POINT('Ctrl Pts',(3.1657847553136,2.84862442585768,-2.6764535284648));
#22586=CARTESIAN_POINT('Ctrl Pts',(3.25036360752406,2.84862442585768,-2.48072272386991));
#22587=CARTESIAN_POINT('Ctrl Pts',(3.32623874336682,2.84862442728679,-2.29790849584301));
#22588=CARTESIAN_POINT('Ctrl Pts',(3.4754687298166,2.84862442728679,-1.91583243746613));
#22589=CARTESIAN_POINT('Ctrl Pts',(3.54997746960448,2.84862442585767,-1.71136210930917));
#22590=CARTESIAN_POINT('Ctrl Pts',(3.61626248314343,2.84862442585767,-1.50713517738359));
#22591=CARTESIAN_POINT('',(3.02384907614375,2.84862442585767,-2.71179421793157));
#22592=CARTESIAN_POINT('',(11.0238490761438,2.84862442585767,-2.71179421793157));
#22593=CARTESIAN_POINT('',(3.02384907614375,2.84862442585767,2.11350930841789));
#22594=CARTESIAN_POINT('',(3.02384907614375,2.84862442585767,1.40404227860195));
#22595=CARTESIAN_POINT('',(3.27104142627809,2.84862444224244,2.71179420072006));
#22596=CARTESIAN_POINT('Ctrl Pts',(3.27100497985698,2.84862442585767,2.71079938718163));
#22597=CARTESIAN_POINT('Ctrl Pts',(3.228076353399,2.84862442585767,2.61225572759565));
#22598=CARTESIAN_POINT('Ctrl Pts',(3.18578823704266,2.84862442598707,2.51303020389064));
#22599=CARTESIAN_POINT('Ctrl Pts',(3.10334913028736,2.84862442598707,2.31421002248986));
#22600=CARTESIAN_POINT('Ctrl Pts',(3.06291723376633,2.84862442585767,2.21392684695503));
#22601=CARTESIAN_POINT('Ctrl Pts',(3.02384907614376,2.84862442585767,2.11350930841789));
#22602=CARTESIAN_POINT('',(3.45436586621803,2.84686430560626,2.71031653510883));
#22603=CARTESIAN_POINT('',(11.0238490761438,2.84862442585767,2.71179421793157));
#22604=CARTESIAN_POINT('',(3.80988877059788,2.84862442585767,1.5071351773836));
#22605=CARTESIAN_POINT('Ctrl Pts',(3.80988877059788,2.84862442585767,1.5071351773836));
#22606=CARTESIAN_POINT('Ctrl Pts',(3.7658293274531,2.84862442585767,1.71164808388438));
#22607=CARTESIAN_POINT('Ctrl Pts',(3.7118046719511,2.84862442781797,1.9153406753387));
#22608=CARTESIAN_POINT('Ctrl Pts',(3.59671531847852,2.84862442781797,2.29823125790659));
#22609=CARTESIAN_POINT('Ctrl Pts',(3.53585880786088,2.84862442585766,2.48068659685609));
#22610=CARTESIAN_POINT('Ctrl Pts',(3.46586775948282,2.84862442585766,2.67641846844891));
#22611=CARTESIAN_POINT('Ctrl Pts',(3.46006601698536,2.84862442585767,2.69254416467973));
#22612=CARTESIAN_POINT('Ctrl Pts',(3.45423416535493,2.84862442585767,2.7086578664456));
#22613=CARTESIAN_POINT('',(4.05643566914408,2.84862442585766,1.50713517738361));
#22614=CARTESIAN_POINT('',(13.3346225254169,2.84862442585767,1.50713517738359));
#22615=CARTESIAN_POINT('',(4.52103878553064,2.84685468828742,2.71031082423224));
#22616=CARTESIAN_POINT('Ctrl Pts',(4.52090646241579,2.84862442585767,2.70864536656847));
#22617=CARTESIAN_POINT('Ctrl Pts',(4.51389718302579,2.84862442585767,2.69253952221217));
#22618=CARTESIAN_POINT('Ctrl Pts',(4.50690787077022,2.84862442585768,2.67642347934393));
#22619=CARTESIAN_POINT('Ctrl Pts',(4.42232697249459,2.84862442585768,2.48069113060106));
#22620=CARTESIAN_POINT('Ctrl Pts',(4.34645166843461,2.84862442738707,2.29787949083546));
#22621=CARTESIAN_POINT('Ctrl Pts',(4.19722448429369,2.84862442738707,1.91581561039782));
#22622=CARTESIAN_POINT('Ctrl Pts',(4.12271784469148,2.84862442585767,1.7113533653371));
#22623=CARTESIAN_POINT('Ctrl Pts',(4.05643566914409,2.84862442585767,1.50713517738361));
#22624=CARTESIAN_POINT('',(4.70436582446518,2.84685313164041,2.71030989474673));
#22625=CARTESIAN_POINT('',(11.0238490761438,2.84862442585767,2.71179421793157));
#22626=CARTESIAN_POINT('',(5.05988877059788,2.84862442585767,1.5071351773836));
#22627=CARTESIAN_POINT('Ctrl Pts',(5.05988877059787,2.84862442585767,1.50713517738362));
#22628=CARTESIAN_POINT('Ctrl Pts',(5.01582936546295,2.84862442585767,1.71164790745213));
#22629=CARTESIAN_POINT('Ctrl Pts',(4.96180378091768,2.84862442783138,1.91534068528627));
#22630=CARTESIAN_POINT('Ctrl Pts',(4.84671331029461,2.84862442783138,2.29822778278234));
#22631=CARTESIAN_POINT('Ctrl Pts',(4.78585648120188,2.84862442585767,2.48068049652974));
#22632=CARTESIAN_POINT('Ctrl Pts',(4.71586588068668,2.84862442585767,2.6764075700122));
#22633=CARTESIAN_POINT('Ctrl Pts',(4.71006469178374,2.84862442585767,2.69253144678897));
#22634=CARTESIAN_POINT('Ctrl Pts',(4.70423340021296,2.84862442585767,2.70864333135427));
#22635=CARTESIAN_POINT('',(5.30643566914408,2.84862442585766,1.50713517738361));
#22636=CARTESIAN_POINT('',(13.3346225254169,2.84862442585767,1.50713517738359));
#22637=CARTESIAN_POINT('',(5.77103875631455,2.8468445755701,2.71030475869924));
#22638=CARTESIAN_POINT('Ctrl Pts',(5.77090577394363,2.84862442585767,2.70863208133986));
#22639=CARTESIAN_POINT('Ctrl Pts',(5.7638971201788,2.84862442585767,2.69252787095137));
#22640=CARTESIAN_POINT('Ctrl Pts',(5.75690842970124,2.84862442585768,2.67641346374591));
#22641=CARTESIAN_POINT('Ctrl Pts',(5.67232833961162,2.84862442585768,2.48068550687512));
#22642=CARTESIAN_POINT('Ctrl Pts',(5.59645299018697,2.84862442739611,2.29787621515313));
#22643=CARTESIAN_POINT('Ctrl Pts',(5.44722527981436,2.84862442739611,1.91581567641076));
#22644=CARTESIAN_POINT('Ctrl Pts',(5.3727177753678,2.84862442585767,1.71135315174791));
#22645=CARTESIAN_POINT('Ctrl Pts',(5.30643566914408,2.84862442585767,1.5071351773836));
#22646=CARTESIAN_POINT('',(5.95436579715553,2.84684318562971,2.71030391984611));
#22647=CARTESIAN_POINT('',(11.0238490761438,2.84862442585767,2.71179421793157));
#22648=CARTESIAN_POINT('',(6.30988877059788,2.84862442585767,1.5071351773836));
#22649=CARTESIAN_POINT('Ctrl Pts',(6.30988877059789,2.84862442585767,1.5071351773836));
#22650=CARTESIAN_POINT('Ctrl Pts',(6.2658293983268,2.84862442585767,1.71164775490643));
#22651=CARTESIAN_POINT('Ctrl Pts',(6.21180298721187,2.84862442784341,1.91534068936543));
#22652=CARTESIAN_POINT('Ctrl Pts',(6.09671151624063,2.84862442784341,2.29822465435504));
#22653=CARTESIAN_POINT('Ctrl Pts',(6.03585440555947,2.84862442585767,2.48067499299047));
#22654=CARTESIAN_POINT('Ctrl Pts',(5.96586420541966,2.84862442585767,2.67639774691987));
#22655=CARTESIAN_POINT('Ctrl Pts',(5.96006351303068,2.84862442585767,2.69251999018277));
#22656=CARTESIAN_POINT('Ctrl Pts',(5.95423272375062,2.84862442585767,2.70863024324505));
#22657=CARTESIAN_POINT('',(6.55643566914408,2.84862442585766,1.50713517738361));
#22658=CARTESIAN_POINT('',(13.3346225254169,2.84862442585767,1.50713517738359));
#22659=CARTESIAN_POINT('',(7.02103873887505,2.84683552060301,2.71029927000383));
#22660=CARTESIAN_POINT('Ctrl Pts',(7.02090516150519,2.84862442585767,2.70862005097967));
#22661=CARTESIAN_POINT('Ctrl Pts',(7.01389707152942,2.84862442585767,2.69251731541987));
#22662=CARTESIAN_POINT('Ctrl Pts',(7.0069089413909,2.84862442585767,2.67640438456248));
#22663=CARTESIAN_POINT('Ctrl Pts',(6.92232957528187,2.84862442585767,2.48068040331129));
#22664=CARTESIAN_POINT('Ctrl Pts',(6.84645418560907,2.84862442740432,2.29787324819636));
#22665=CARTESIAN_POINT('Ctrl Pts',(6.6972259948484,2.84862442740432,1.91581572986742));
#22666=CARTESIAN_POINT('Ctrl Pts',(6.62271771463721,2.84862442585767,1.71135296463439));
#22667=CARTESIAN_POINT('Ctrl Pts',(6.55643566914408,2.84862442585767,1.5071351773836));
#22668=CARTESIAN_POINT('',(7.20436578122244,2.84683427137383,2.71029850822801));
#22669=CARTESIAN_POINT('',(11.0238490761438,2.84862442585767,2.71179421793157));
#22670=CARTESIAN_POINT('',(7.55988877059788,2.84862442585767,1.5071351773836));
#22671=CARTESIAN_POINT('Ctrl Pts',(7.55988877059788,2.84862442585767,1.5071351773836));
#22672=CARTESIAN_POINT('Ctrl Pts',(7.51582942694069,2.84862442585767,1.71164762208787));
#22673=CARTESIAN_POINT('Ctrl Pts',(7.46180227524923,2.84862442785429,1.91534068886327));
#22674=CARTESIAN_POINT('Ctrl Pts',(7.34670990240678,2.84862442785429,2.29822181949426));
#22675=CARTESIAN_POINT('Ctrl Pts',(7.28585254096374,2.84862442585767,2.48066999572136));
#22676=CARTESIAN_POINT('Ctrl Pts',(7.2158627012126,2.84862442585767,2.67638883532302));
#22677=CARTESIAN_POINT('Ctrl Pts',(7.21006245715211,2.84862442585767,2.69250960216246));
#22678=CARTESIAN_POINT('Ctrl Pts',(7.20423212139549,2.84862442585767,2.70861838061489));
#22679=CARTESIAN_POINT('',(7.80643566914408,2.84862442585766,1.50713517738361));
#22680=CARTESIAN_POINT('',(13.3346225254169,2.84862442585767,1.50713517738359));
#22681=CARTESIAN_POINT('',(8.271038730764,2.84682736201001,2.71029427388594));
#22682=CARTESIAN_POINT('Ctrl Pts',(8.27090461316402,2.84862442585767,2.70860909277273));
#22683=CARTESIAN_POINT('Ctrl Pts',(8.26389703435909,2.84862442585767,2.69250769644918));
#22684=CARTESIAN_POINT('Ctrl Pts',(8.25690941227972,2.84862442585767,2.67639610620256));
#22685=CARTESIAN_POINT('Ctrl Pts',(8.17233069882605,2.84862442585767,2.48067574504101));
#22686=CARTESIAN_POINT('Ctrl Pts',(8.0964552732107,2.84862442741179,2.29787054506796));
#22687=CARTESIAN_POINT('Ctrl Pts',(7.94722664153419,2.84862442741179,1.91581577309339));
#22688=CARTESIAN_POINT('Ctrl Pts',(7.87271766108794,2.84862442585767,1.71135279964682));
#22689=CARTESIAN_POINT('Ctrl Pts',(7.80643566914409,2.84862442585767,1.50713517738362));
#22690=CARTESIAN_POINT('',(8.45436577430856,2.84682623267637,2.71029357829656));
#22691=CARTESIAN_POINT('',(11.0238490761438,2.84862442585767,2.71179421793157));
#22692=CARTESIAN_POINT('',(8.80988877059788,2.84862442585767,1.50713517738359));
#22693=CARTESIAN_POINT('Ctrl Pts',(8.80988877059788,2.84862442585767,1.50713517738359));
#22694=CARTESIAN_POINT('Ctrl Pts',(8.76582945201024,2.84862442585767,1.7116475057213));
#22695=CARTESIAN_POINT('Ctrl Pts',(8.71180163264592,2.84862442786418,1.91534068476964));
#22696=CARTESIAN_POINT('Ctrl Pts',(8.59670844181264,2.84862442786418,2.29821923576154));
#22697=CARTESIAN_POINT('Ctrl Pts',(8.53585085563285,2.84862442585767,2.48066543233191));
#22698=CARTESIAN_POINT('Ctrl Pts',(8.46586134225275,2.84862442585767,2.67638070425965));
#22699=CARTESIAN_POINT('Ctrl Pts',(8.46006150542514,2.84862442585767,2.69250012875935));
#22700=CARTESIAN_POINT('Ctrl Pts',(8.45423158160217,2.84862442585767,2.70860756651644));
#22701=CARTESIAN_POINT('',(9.05643566914408,2.84862442585766,1.50713517738361));
#22702=CARTESIAN_POINT('',(13.3346225254169,2.84862442585767,1.50713517738359));
#22703=CARTESIAN_POINT('',(9.52103873008012,2.84681996992432,2.71028970229123));
#22704=CARTESIAN_POINT('Ctrl Pts',(9.52090411935796,2.84862442585767,2.70859905909218));
#22705=CARTESIAN_POINT('Ctrl Pts',(9.51389700653417,2.84862442585767,2.69249888540408));
#22706=CARTESIAN_POINT('Ctrl Pts',(9.50690984761346,2.84862442585768,2.67638851904301));
#22707=CARTESIAN_POINT('Ctrl Pts',(9.42233172583661,2.84862442585768,2.48067147148852));
#22708=CARTESIAN_POINT('Ctrl Pts',(9.3464562679359,2.84862442741865,2.29786806948615));
#22709=CARTESIAN_POINT('Ctrl Pts',(9.19722722963917,2.84862442741865,1.9158158079193));
#22710=CARTESIAN_POINT('Ctrl Pts',(9.12271761359435,2.84862442585767,1.71135265331708));
#22711=CARTESIAN_POINT('Ctrl Pts',(9.05643566914409,2.84862442585767,1.50713517738362));
#22712=CARTESIAN_POINT('',(9.70436577458009,2.8468189436181,2.71028906402778));
#22713=CARTESIAN_POINT('',(11.0238490761438,2.84862442585767,2.71179421793157));
#22714=CARTESIAN_POINT('',(10.0598887705979,2.84862442585767,1.50713517738359));
#22715=CARTESIAN_POINT('Ctrl Pts',(10.0598887705979,2.84862442585767,1.50713517738359));
#22716=CARTESIAN_POINT('Ctrl Pts',(10.0158294740978,2.84862442585767,1.71164740319615));
#22717=CARTESIAN_POINT('Ctrl Pts',(9.96180104943227,2.84862442787322,1.91534067785543));
#22718=CARTESIAN_POINT('Ctrl Pts',(9.84670711270893,2.84862442787322,2.29821686881042));
#22719=CARTESIAN_POINT('Ctrl Pts',(9.78584932396424,2.84862442585767,2.48066124415883));
#22720=CARTESIAN_POINT('Ctrl Pts',(9.71586010775059,2.84862442585767,2.67637324766241));
#22721=CARTESIAN_POINT('Ctrl Pts',(9.71006064278651,2.84862442585767,2.69249144531452));
#22722=CARTESIAN_POINT('Ctrl Pts',(9.70423109510515,2.84862442585767,2.70859765771964));
#22723=CARTESIAN_POINT('',(10.3064356691441,2.84862442585766,1.50713517738361));
#22724=CARTESIAN_POINT('',(13.3346225254169,2.84862442585767,1.50713517738359));
#22725=CARTESIAN_POINT('',(10.771038735331,2.84681323863445,2.71028549959174));
#22726=CARTESIAN_POINT('Ctrl Pts',(10.7709036723368,2.84862442585767,2.70858982922371));
#22727=CARTESIAN_POINT('Ctrl Pts',(10.7638969863635,2.84862442585767,2.69249077707409));
#22728=CARTESIAN_POINT('Ctrl Pts',(10.7569102517173,2.84862442585767,2.67638153338721));
#22729=CARTESIAN_POINT('Ctrl Pts',(10.6723326690498,2.84862442585767,2.48066753305333));
#22730=CARTESIAN_POINT('Ctrl Pts',(10.5964571819956,2.84862442742496,2.29786579177956));
#22731=CARTESIAN_POINT('Ctrl Pts',(10.4472277671172,2.84862442742496,1.91581583580293));
#22732=CARTESIAN_POINT('Ctrl Pts',(10.3727175712488,2.84862442585767,1.71135252284851));
#22733=CARTESIAN_POINT('Ctrl Pts',(10.3064356691441,2.84862442585767,1.5071351773836));
#22734=CARTESIAN_POINT('',(10.9543681768003,2.84860418144656,2.71177492056083));
#22735=CARTESIAN_POINT('',(11.0238490761438,2.84862442585767,2.71179421793157));
#22736=CARTESIAN_POINT('',(11.0238490761438,2.84862442585767,2.5145657703754));
#22737=CARTESIAN_POINT('Ctrl Pts',(11.0238490761438,2.84862442585767,2.51456577037539));
#22738=CARTESIAN_POINT('Ctrl Pts',(11.0125388019847,2.84862442585767,2.54755700411209));
#22739=CARTESIAN_POINT('Ctrl Pts',(11.0010794330984,2.84862442585774,2.58050639119045));
#22740=CARTESIAN_POINT('Ctrl Pts',(10.9781080325486,2.84862442585774,2.6456791051022));
#22741=CARTESIAN_POINT('Ctrl Pts',(10.9665953160741,2.84862442585767,2.67792052124666));
#22742=CARTESIAN_POINT('Ctrl Pts',(10.9547630945647,2.84862442585767,2.71065726237697));
#22743=CARTESIAN_POINT('Ctrl Pts',(10.9545649113151,2.84862442585767,2.71120547217373));
#22744=CARTESIAN_POINT('Ctrl Pts',(10.9543666920789,2.84862442585767,2.71175366890678));
#22745=CARTESIAN_POINT('',(11.0238490761438,2.84862442585767,-6.75363122348402));
#22746=CARTESIAN_POINT('Origin',(13.3346225254169,0.,0.));
#22747=CARTESIAN_POINT('',(3.02386560100257,-0.0279675576018124,3.22262864416951));
#22748=CARTESIAN_POINT('Ctrl Pts',(3.23780938168963,-2.84862442585767,1.50713517738358));
#22749=CARTESIAN_POINT('Ctrl Pts',(3.2313463182794,-2.79966227599299,1.5996781543773));
#22750=CARTESIAN_POINT('Ctrl Pts',(3.22488325486918,-2.74617683440501,1.68985168048399));
#22751=CARTESIAN_POINT('Ctrl Pts',(3.21842019145895,-2.68842250870076,1.77721748168622));
#22752=CARTESIAN_POINT('Ctrl Pts',(3.21195831309532,-2.63067877264464,1.86456726377506));
#22753=CARTESIAN_POINT('Ctrl Pts',(3.20549643473169,-2.56866791940005,1.94911003510213));
#22754=CARTESIAN_POINT('Ctrl Pts',(3.19903455636806,-2.50268804578698,2.03043594037708));
#22755=CARTESIAN_POINT('Ctrl Pts',(3.19257306896931,-2.43671216417302,2.11175692516759));
#22756=CARTESIAN_POINT('Ctrl Pts',(3.18611158157055,-2.36676797758294,2.18986114188401));
#22757=CARTESIAN_POINT('Ctrl Pts',(3.17965009417179,-2.29319407993019,2.26437154068698));
#22758=CARTESIAN_POINT('Ctrl Pts',(3.17318610757495,-2.2195917250922,2.33891075889858));
#22759=CARTESIAN_POINT('Ctrl Pts',(3.16672212097811,-2.14235711490485,2.409853112714));
#22760=CARTESIAN_POINT('Ctrl Pts',(3.16025813438127,-2.06186607637872,2.47685805923121));
#22761=CARTESIAN_POINT('Ctrl Pts',(3.15379347444796,-1.98136665331285,2.54386998547744));
#22762=CARTESIAN_POINT('Ctrl Pts',(3.14732881451464,-1.89761041744266,2.60694345163933));
#22763=CARTESIAN_POINT('Ctrl Pts',(3.14086415458132,-1.81100596096446,2.66577849264548));
#22764=CARTESIAN_POINT('Ctrl Pts',(3.13439513068962,-1.72434304228595,2.72465325015229));
#22765=CARTESIAN_POINT('Ctrl Pts',(3.12792610679791,-1.63482837237314,2.77928365617125));
#22766=CARTESIAN_POINT('Ctrl Pts',(3.12145708290621,-1.54289948435689,2.82941314474773));
#22767=CARTESIAN_POINT('Ctrl Pts',(3.11566378858085,-1.46057313741543,2.87430629811445));
#22768=CARTESIAN_POINT('Ctrl Pts',(3.1098704942555,-1.37631113062514,2.91559022856466));
#22769=CARTESIAN_POINT('Ctrl Pts',(3.10407719993014,-1.29044359936636,2.9531124054723));
#22770=CARTESIAN_POINT('Ctrl Pts',(3.09739290001951,-1.19136968748049,2.99640547322698));
#22771=CARTESIAN_POINT('Ctrl Pts',(3.09070860010888,-1.0900490626428,3.03473683538019));
#22772=CARTESIAN_POINT('Ctrl Pts',(3.08402430019824,-0.987005187934864,
3.06788825114111));
#22773=CARTESIAN_POINT('Ctrl Pts',(3.07764680269255,-0.8886909197672,3.09951805144215));
#22774=CARTESIAN_POINT('Ctrl Pts',(3.07126930518686,-0.788808504705706,
3.12643274001858));
#22775=CARTESIAN_POINT('Ctrl Pts',(3.06489180768116,-0.687831587946816,
3.14849253915625));
#22776=CARTESIAN_POINT('Ctrl Pts',(3.05851704894084,-0.586898034918329,
3.17054286488937));
#22777=CARTESIAN_POINT('Ctrl Pts',(3.05214229020051,-0.484871300248373,
3.18774237030377));
#22778=CARTESIAN_POINT('Ctrl Pts',(3.04576753146018,-0.382237297735694,
3.20000190792439));
#22779=CARTESIAN_POINT('Ctrl Pts',(3.03939415566387,-0.279625560705552,
3.2122587859535));
#22780=CARTESIAN_POINT('Ctrl Pts',(3.03302077986756,-0.176407208550043,
3.2195777843509));
#22781=CARTESIAN_POINT('Ctrl Pts',(3.02664740407124,-0.0730749405909518,
3.22192141672599));
#22782=CARTESIAN_POINT('Ctrl Pts',(3.02572013638169,-0.0580410438885451,
3.22226239372893));
#22783=CARTESIAN_POINT('Ctrl Pts',(3.02479286869213,-0.0430047421599852,
3.22249814408038));
#22784=CARTESIAN_POINT('Ctrl Pts',(3.02386560100257,-0.0279675576018124,
3.22262864416951));
#22785=CARTESIAN_POINT('Origin',(3.02384907614375,0.,0.));
#22786=CARTESIAN_POINT('Origin',(13.3346225254169,0.,0.));
#22787=CARTESIAN_POINT('Ctrl Pts',(3.61626248314343,2.84862442585767,-1.50713517738359));
#22788=CARTESIAN_POINT('Ctrl Pts',(3.60981814030002,2.79980409716038,-1.59941009929665));
#22789=CARTESIAN_POINT('Ctrl Pts',(3.6033737974566,2.74648418316931,-1.68933387103504));
#22790=CARTESIAN_POINT('Ctrl Pts',(3.59692945461318,2.68891651929892,-1.77646995886263));
#22791=CARTESIAN_POINT('Ctrl Pts',(3.59048653183097,2.63136154091221,-1.86358684557373));
#22792=CARTESIAN_POINT('Ctrl Pts',(3.58404360904876,2.56956088675986,-1.94791695677699));
#22793=CARTESIAN_POINT('Ctrl Pts',(3.57760068626655,2.50381017084846,-2.02905204242173));
#22794=CARTESIAN_POINT('Ctrl Pts',(3.57115830034015,2.438064933608,-2.11018036749468));
#22795=CARTESIAN_POINT('Ctrl Pts',(3.56471591441375,2.36837052961789,-2.1881139039722));
#22796=CARTESIAN_POINT('Ctrl Pts',(3.55827352848734,2.29506314790585,-2.26247711803335));
#22797=CARTESIAN_POINT('Ctrl Pts',(3.5518307966975,2.22175183064207,-2.33684432432924));
#22798=CARTESIAN_POINT('Ctrl Pts',(3.54538806490766,2.14482741599023,-2.40764055767011));
#22799=CARTESIAN_POINT('Ctrl Pts',(3.53894533311782,2.06466301231591,-2.47452706755748));
#22800=CARTESIAN_POINT('Ctrl Pts',(3.53249922680016,1.9844566207056,-2.54144861078092));
#22801=CARTESIAN_POINT('Ctrl Pts',(3.52605312048251,1.90100714009866,-2.60445609580204));
#22802=CARTESIAN_POINT('Ctrl Pts',(3.51960701416485,1.81472094286566,-2.66325091983928));
#22803=CARTESIAN_POINT('Ctrl Pts',(3.51315938360299,1.72841434242652,-2.72205964648149));
#22804=CARTESIAN_POINT('Ctrl Pts',(3.50671175304113,1.63927000535803,-2.77665351913181));
#22805=CARTESIAN_POINT('Ctrl Pts',(3.50026412247928,1.54772264342607,-2.82677770288472));
#22806=CARTESIAN_POINT('Ctrl Pts',(3.49381173810022,1.45610778391972,-2.87693884303648));
#22807=CARTESIAN_POINT('Ctrl Pts',(3.48735935372116,1.36208669566401,-2.92262353462528));
#22808=CARTESIAN_POINT('Ctrl Pts',(3.4809069693421,1.26611816796091,-2.96362317902586));
#22809=CARTESIAN_POINT('Ctrl Pts',(3.47809506143749,1.22429569648526,-2.9814905622138));
#22810=CARTESIAN_POINT('Ctrl Pts',(3.47528315353287,1.18210364055045,-2.99846879411564));
#22811=CARTESIAN_POINT('Ctrl Pts',(3.47247124562825,1.1395810861412,-3.0145434995384));
#22812=CARTESIAN_POINT('Ctrl Pts',(3.46617126457528,1.04431079415822,-3.05055831333412));
#22813=CARTESIAN_POINT('Ctrl Pts',(3.45987128352231,0.947252186086576,-3.08208279945663));
#22814=CARTESIAN_POINT('Ctrl Pts',(3.45357130246934,0.848856252778096,-3.10894847571));
#22815=CARTESIAN_POINT('Ctrl Pts',(3.44727552762368,0.750526013904431,-3.13579621498815));
#22816=CARTESIAN_POINT('Ctrl Pts',(3.44097975277802,0.650860620899843,-3.15799122523729));
#22817=CARTESIAN_POINT('Ctrl Pts',(3.43468397793237,0.550327087937376,-3.17541456486903));
#22818=CARTESIAN_POINT('Ctrl Pts',(3.42839100102228,0.449838233565586,-3.19283016131065));
#22819=CARTESIAN_POINT('Ctrl Pts',(3.42209802411218,0.348482410725096,-3.20547823762093));
#22820=CARTESIAN_POINT('Ctrl Pts',(3.41580504720209,0.246737031113831,-3.21329089874806));
#22821=CARTESIAN_POINT('Ctrl Pts',(3.40951346280697,0.14501416580161,-3.22110183108329));
#22822=CARTESIAN_POINT('Ctrl Pts',(3.40322187841185,0.0429023241629521,
-3.22407944781139));
#22823=CARTESIAN_POINT('Ctrl Pts',(3.39693029401672,-0.0591164460693605,
-3.22220775374651));
#22824=CARTESIAN_POINT('Ctrl Pts',(3.39063656516385,-0.161169988932681,
-3.22033542172327));
#22825=CARTESIAN_POINT('Ctrl Pts',(3.38434283631098,-0.263129986453162,
-3.21361047975511));
#22826=CARTESIAN_POINT('Ctrl Pts',(3.3780491074581,-0.36451508727217,-3.20206906759535));
#22827=CARTESIAN_POINT('Ctrl Pts',(3.37175438206171,-0.465916241319268,
-3.1905258279785));
#22828=CARTESIAN_POINT('Ctrl Pts',(3.36545965666533,-0.566741910482421,
-3.17416465359994));
#22829=CARTESIAN_POINT('Ctrl Pts',(3.35916493126894,-0.666517837287942,
-3.15307334755743));
#22830=CARTESIAN_POINT('Ctrl Pts',(3.3528648162117,-0.766379194095918,-3.13196398274679));
#22831=CARTESIAN_POINT('Ctrl Pts',(3.34656470115446,-0.865188613006443,
-3.10611648897175));
#22832=CARTESIAN_POINT('Ctrl Pts',(3.34026458609723,-0.962483988941134,
-3.07566937975003));
#22833=CARTESIAN_POINT('Ctrl Pts',(3.33640306010251,-1.02211918923905,-3.05700745014149));
#22834=CARTESIAN_POINT('Ctrl Pts',(3.33254153410778,-1.0811858773422,-3.03661850873259));
#22835=CARTESIAN_POINT('Ctrl Pts',(3.32868000811306,-1.13958108614105,-3.01454349953846));
#22836=CARTESIAN_POINT('Ctrl Pts',(3.32222787133228,-1.23715232482427,-2.97765886404663));
#22837=CARTESIAN_POINT('Ctrl Pts',(3.31577573455149,-1.33298225140899,-2.93601378761227));
#22838=CARTESIAN_POINT('Ctrl Pts',(3.30932359777071,-1.42660369135491,-2.8897957488917));
#22839=CARTESIAN_POINT('Ctrl Pts',(3.30287533190599,-1.52016896374772,-2.84360543837256));
#22840=CARTESIAN_POINT('Ctrl Pts',(3.29642706604126,-1.61152805019238,-2.79284779845975));
#22841=CARTESIAN_POINT('Ctrl Pts',(3.28997880017654,-1.70023542039651,-2.73775767330293));
#22842=CARTESIAN_POINT('Ctrl Pts',(3.28353351658572,-1.78890176411679,-2.68269302690989));
#22843=CARTESIAN_POINT('Ctrl Pts',(3.2770882329949,-1.87491851400246,-2.6233000873556));
#22844=CARTESIAN_POINT('Ctrl Pts',(3.27064294940408,-1.95786663758549,-2.55985854920339));
#22845=CARTESIAN_POINT('Ctrl Pts',(3.26419976213879,-2.04078778232953,-2.49643764538225));
#22846=CARTESIAN_POINT('Ctrl Pts',(3.25775657487349,-2.12064198953114,-2.42897099735954));
#22847=CARTESIAN_POINT('Ctrl Pts',(3.25131338760819,-2.19704128404677,-2.35778013366262));
#22848=CARTESIAN_POINT('Ctrl Pts',(3.24487046796784,-2.27343740523273,-2.2865922269574));
#22849=CARTESIAN_POINT('Ctrl Pts',(3.23842754832749,-2.34637861930785,-2.21168066725837));
#22850=CARTESIAN_POINT('Ctrl Pts',(3.23198462868714,-2.41551206945869,-2.13340549469607));
#22851=CARTESIAN_POINT('Ctrl Pts',(3.22554227911908,-2.48463940265226,-2.05513724795456));
#22852=CARTESIAN_POINT('Ctrl Pts',(3.21909992955102,-2.54995939553337,-1.97350626776285));
#22853=CARTESIAN_POINT('Ctrl Pts',(3.21265757998296,-2.6111583393268,-1.88890700921568));
#22854=CARTESIAN_POINT('Ctrl Pts',(3.20621358079725,-2.67237295362312,-1.80428608831874));
#22855=CARTESIAN_POINT('Ctrl Pts',(3.19976958161155,-2.72946418966193,-1.71669567822796));
#22856=CARTESIAN_POINT('Ctrl Pts',(3.19332558242584,-2.78216069558516,-1.62656061259366));
#22857=CARTESIAN_POINT('Ctrl Pts',(3.19051331181652,-2.80515834511165,-1.58722414021874));
#22858=CARTESIAN_POINT('Ctrl Pts',(3.1877010412072,-2.82731954204425,-1.54740337185725));
#22859=CARTESIAN_POINT('Ctrl Pts',(3.18488877059788,-2.84862442585766,-1.50713517738361));
#22860=CARTESIAN_POINT('Ctrl Pts',(3.86280938168963,2.84862442585768,-1.50713517738357));
#22861=CARTESIAN_POINT('Ctrl Pts',(3.85636606854818,2.79981189786092,-1.5993953552535));
#22862=CARTESIAN_POINT('Ctrl Pts',(3.84992275540674,2.74650107987591,-1.6893054006252));
#22863=CARTESIAN_POINT('Ctrl Pts',(3.84347944226529,2.68894366242018,-1.77642887356357));
#22864=CARTESIAN_POINT('Ctrl Pts',(3.83703756419086,2.63139906426248,-1.86353294219552));
#22865=CARTESIAN_POINT('Ctrl Pts',(3.83059568611644,2.56960996034231,-1.94785135922787));
#22866=CARTESIAN_POINT('Ctrl Pts',(3.82415380804201,2.50387182458097,-2.02897596056966));
#22867=CARTESIAN_POINT('Ctrl Pts',(3.81771247715649,2.43813927277788,-2.11009367098914));
#22868=CARTESIAN_POINT('Ctrl Pts',(3.81127114627096,2.36845859682568,-2.18801781258259));
#22869=CARTESIAN_POINT('Ctrl Pts',(3.80482981538543,2.29516584988645,-2.2623729321257));
#22870=CARTESIAN_POINT('Ctrl Pts',(3.79838814430917,2.22186923208361,-2.33673197864027));
#22871=CARTESIAN_POINT('Ctrl Pts',(3.79194647323291,2.14496043015097,-2.40752135873283));
#22872=CARTESIAN_POINT('Ctrl Pts',(3.78550480215665,2.06481241972296,-2.47440239933965));
#22873=CARTESIAN_POINT('Ctrl Pts',(3.77905975356884,1.98462238590886,-2.54131850716494));
#22874=CARTESIAN_POINT('Ctrl Pts',(3.77261470498103,1.90119004104676,-2.60432193774656));
#22875=CARTESIAN_POINT('Ctrl Pts',(3.76616965639323,1.81492162709215,-2.66311416390908));
#22876=CARTESIAN_POINT('Ctrl Pts',(3.75972307966444,1.72863275862937,-2.72192032989055));
#22877=CARTESIAN_POINT('Ctrl Pts',(3.75327650293565,1.63950679792908,-2.77651309360132));
#22878=CARTESIAN_POINT('Ctrl Pts',(3.74682992620685,1.54797832620639,-2.82663769593757));
#22879=CARTESIAN_POINT('Ctrl Pts',(3.74037857905811,1.45638212407943,-2.87679939011548));
#22880=CARTESIAN_POINT('Ctrl Pts',(3.73392723190936,1.3623801950629,-2.92248614132501));
#22881=CARTESIAN_POINT('Ctrl Pts',(3.72747588476061,1.26643119723935,-2.96348942720552));
#22882=CARTESIAN_POINT('Ctrl Pts',(3.72465663789856,1.22450136385816,-2.98140791498601));
#22883=CARTESIAN_POINT('Ctrl Pts',(3.7218373910365,1.18219996526355,-2.99843261799755));
#22884=CARTESIAN_POINT('Ctrl Pts',(3.71901814417445,1.13956640274635,-3.0145490502282));
#22885=CARTESIAN_POINT('Ctrl Pts',(3.71271660161073,1.04427243879401,-3.05057228219266));
#22886=CARTESIAN_POINT('Ctrl Pts',(3.706415059047,0.947189762030143,-3.08210278953502));
#22887=CARTESIAN_POINT('Ctrl Pts',(3.70011351648328,0.848769608982329,-3.10897213132701));
#22888=CARTESIAN_POINT('Ctrl Pts',(3.6938161682386,0.750414964580609,-3.13582358883261));
#22889=CARTESIAN_POINT('Ctrl Pts',(3.68751881999391,0.650725009496901,-3.15801994590081));
#22890=CARTESIAN_POINT('Ctrl Pts',(3.68122147174923,0.550166988852229,-3.17544230728213));
#22891=CARTESIAN_POINT('Ctrl Pts',(3.67492691326741,0.449653516011018,-3.19285695045336));
#22892=CARTESIAN_POINT('Ctrl Pts',(3.6686323547856,0.348273146329405,-3.20550173722294));
#22893=CARTESIAN_POINT('Ctrl Pts',(3.66233779630378,0.246503510729632,-3.2133088214017));
#22894=CARTESIAN_POINT('Ctrl Pts',(3.65604462587464,0.144756316992322,-3.22111418399122));
#22895=CARTESIAN_POINT('Ctrl Pts',(3.64975145544551,0.0426204367755807,
-3.22408393729004));
#22896=CARTESIAN_POINT('Ctrl Pts',(3.64345828501638,-0.0594218713400216,
-3.22220213576157));
#22897=CARTESIAN_POINT('Ctrl Pts',(3.63716297451389,-0.161498880251751,
-3.22031969430236));
#22898=CARTESIAN_POINT('Ctrl Pts',(3.63086766401141,-0.263481843224689,
-3.21358240497111));
#22899=CARTESIAN_POINT('Ctrl Pts',(3.62457235350892,-0.364889203980296,
-3.20202645699854));
#22900=CARTESIAN_POINT('Ctrl Pts',(3.61827604930386,-0.466312571691608,
-3.19046868494194));
#22901=CARTESIAN_POINT('Ctrl Pts',(3.61197974509879,-0.567159749635694,
-3.17409079367219));
#22902=CARTESIAN_POINT('Ctrl Pts',(3.60568344089372,-0.666956276636632,
-3.15298063545512));
#22903=CARTESIAN_POINT('Ctrl Pts',(3.59938176457317,-0.766837951757845,
-3.1318524656865));
#22904=CARTESIAN_POINT('Ctrl Pts',(3.59308008825263,-0.86566678543172,-3.10598405634246));
#22905=CARTESIAN_POINT('Ctrl Pts',(3.58677841193208,-0.962980468876425,
-3.07551396990203));
#22906=CARTESIAN_POINT('Ctrl Pts',(3.58292791017447,-1.02244187090388,-3.05689588870818));
#22907=CARTESIAN_POINT('Ctrl Pts',(3.57907740841687,-1.08133787029128,-3.03656072698695));
#22908=CARTESIAN_POINT('Ctrl Pts',(3.57522690665926,-1.13956640274621,-3.01454905022826));
#22909=CARTESIAN_POINT('Ctrl Pts',(3.56877580865339,-1.23712199244632,-2.97767087356899));
#22910=CARTESIAN_POINT('Ctrl Pts',(3.56232471064752,-1.33293715724246,-2.93603367737495));
#22911=CARTESIAN_POINT('Ctrl Pts',(3.55587361264165,-1.4265448349937,-2.88982480372994));
#22912=CARTESIAN_POINT('Ctrl Pts',(3.54942639732379,-1.52009617359032,-2.84364374157368));
#22913=CARTESIAN_POINT('Ctrl Pts',(3.54297918200593,-1.61144233285859,-2.79289665086444));
#22914=CARTESIAN_POINT('Ctrl Pts',(3.53653196668807,-1.70013788545573,-2.73781824322546));
#22915=CARTESIAN_POINT('Ctrl Pts',(3.53008774073388,-1.7887923128152,-2.68276537364941));
#22916=CARTESIAN_POINT('Ctrl Pts',(3.52364351477968,-1.8747982608721,-2.62338538836474));
#22917=CARTESIAN_POINT('Ctrl Pts',(3.51719928882549,-1.95773679325689,-2.55995785333044));
#22918=CARTESIAN_POINT('Ctrl Pts',(3.51075716161945,-2.04064831431511,-2.49655097530337));
#22919=CARTESIAN_POINT('Ctrl Pts',(3.50431503441341,-2.12049411009414,-2.42909940481136));
#22920=CARTESIAN_POINT('Ctrl Pts',(3.49787290720737,-2.19688629710065,-2.35792454504197));
#22921=CARTESIAN_POINT('Ctrl Pts',(3.49143104021728,-2.27327539840822,-2.28675256022876));
#22922=CARTESIAN_POINT('Ctrl Pts',(3.48498917322719,-2.3462108883281,-2.21185784036661));
#22923=CARTESIAN_POINT('Ctrl Pts',(3.47854730623709,-2.4153399985513,-2.13360030321947));
#22924=CARTESIAN_POINT('Ctrl Pts',(3.47210600263395,-2.48446306294354,-2.05534961024896));
#22925=CARTESIAN_POINT('Ctrl Pts',(3.46566469903081,-2.54978016307586,-1.97373697256748));
#22926=CARTESIAN_POINT('Ctrl Pts',(3.45922339542768,-2.61097767827721,-1.88915672352459));
#22927=CARTESIAN_POINT('Ctrl Pts',(3.45278042233379,-2.67219105497052,-1.80455455253053));
#22928=CARTESIAN_POINT('Ctrl Pts',(3.44633744923991,-2.72928249243958,-1.71698354132592));
#22929=CARTESIAN_POINT('Ctrl Pts',(3.43989447614602,-2.78198072685917,-1.6268684021408));
#22930=CARTESIAN_POINT('Ctrl Pts',(3.43707487381204,-2.80504276089236,-1.58743181703159));
#22931=CARTESIAN_POINT('Ctrl Pts',(3.43425527147806,-2.82726399918805,-1.54750835297587));
#22932=CARTESIAN_POINT('Ctrl Pts',(3.43143566914408,-2.84862442585766,-1.50713517738361));
#22933=CARTESIAN_POINT('Origin',(13.3346225254169,0.,0.));
#22934=CARTESIAN_POINT('Ctrl Pts',(4.48780938168963,-2.84862442585767,1.50713517738358));
#22935=CARTESIAN_POINT('Ctrl Pts',(4.48136661099587,-2.79981600727515,1.59938758808176));
#22936=CARTESIAN_POINT('Ctrl Pts',(4.4749238403021,-2.74650998087232,1.68929040254968));
#22937=CARTESIAN_POINT('Ctrl Pts',(4.46848106960834,-2.68895796079644,1.77640723021763));
#22938=CARTESIAN_POINT('Ctrl Pts',(4.46203974188704,-2.63141883051341,1.86350454653112));
#22939=CARTESIAN_POINT('Ctrl Pts',(4.45559841416573,-2.56963581058662,1.94781680342466));
#22940=CARTESIAN_POINT('Ctrl Pts',(4.44915708644443,-2.50390430110695,2.02893588203228));
#22941=CARTESIAN_POINT('Ctrl Pts',(4.44271631136336,-2.43817843112874,2.11004800094636));
#22942=CARTESIAN_POINT('Ctrl Pts',(4.43627553628229,-2.36850498597941,2.18796719366113));
#22943=CARTESIAN_POINT('Ctrl Pts',(4.42983476120122,-2.2952199472197,2.26231804934337));
#22944=CARTESIAN_POINT('Ctrl Pts',(4.42339364893318,-2.22193107184706,2.33667279743611));
#22945=CARTESIAN_POINT('Ctrl Pts',(4.41695253666512,-2.14503049317434,2.40745856738946));
#22946=CARTESIAN_POINT('Ctrl Pts',(4.41051142439708,-2.06489111689294,2.47433672685765));
#22947=CARTESIAN_POINT('Ctrl Pts',(4.404066933082,-1.98470969900286,2.54124997101879));
#22948=CARTESIAN_POINT('Ctrl Pts',(4.39762244176692,-1.90128637962944,2.60425126539633));
#22949=CARTESIAN_POINT('Ctrl Pts',(4.39117795045184,-1.81502733201031,2.663042122565));
#22950=CARTESIAN_POINT('Ctrl Pts',(4.38473192897104,-1.72874780323421,2.72184693890444));
#22951=CARTESIAN_POINT('Ctrl Pts',(4.37828590749023,-1.63963152143695,2.77643911766918));
#22952=CARTESIAN_POINT('Ctrl Pts',(4.37183988600943,-1.54811299905293,2.82656393960288));
#22953=CARTESIAN_POINT('Ctrl Pts',(4.3653890854091,-1.45652662427993,2.87672592438435));
#22954=CARTESIAN_POINT('Ctrl Pts',(4.35893828480877,-1.36253478677607,2.922413759257));
#22955=CARTESIAN_POINT('Ctrl Pts',(4.35248748420844,-1.26659607549749,2.96341896194824));
#22956=CARTESIAN_POINT('Ctrl Pts',(4.34966437086378,-1.2246096814262,2.98136438331384));
#22957=CARTESIAN_POINT('Ctrl Pts',(4.34684125751911,-1.18225067630238,2.99841357392487));
#22958=CARTESIAN_POINT('Ctrl Pts',(4.34401814417444,-1.13955862823483,3.01455198915453));
#22959=CARTESIAN_POINT('Ctrl Pts',(4.33771576978968,-1.04425205094761,3.05057970832007));
#22960=CARTESIAN_POINT('Ctrl Pts',(4.33141339540492,-0.94715654926464,3.08211342543778));
#22961=CARTESIAN_POINT('Ctrl Pts',(4.32511102102016,-0.848723490673857,
3.10898472155757));
#22962=CARTESIAN_POINT('Ctrl Pts',(4.31881283459272,-0.750355841312021,
3.1358381615751));
#22963=CARTESIAN_POINT('Ctrl Pts',(4.31251464816528,-0.650652797700703,
3.15803523728402));
#22964=CARTESIAN_POINT('Ctrl Pts',(4.30621646173785,-0.550081728076085,
3.17545707811282));
#22965=CARTESIAN_POINT('Ctrl Pts',(4.29992106070215,-0.44955513630709,3.19287121408053));
#22966=CARTESIAN_POINT('Ctrl Pts',(4.29362565966646,-0.348161685766163,
3.20551424845805));
#22967=CARTESIAN_POINT('Ctrl Pts',(4.28733025863076,-0.246379124247223,
3.21331836107709));
#22968=CARTESIAN_POINT('Ctrl Pts',(4.2810362432644,-0.14461896590384,3.22112075594702));
#22969=CARTESIAN_POINT('Ctrl Pts',(4.27474222789805,-0.0424702754849352,
3.22408631900469));
#22970=CARTESIAN_POINT('Ctrl Pts',(4.26844821253169,0.0595845760164542,
3.22219913115266));
#22971=CARTESIAN_POINT('Ctrl Pts',(4.26215205943878,0.161674089868234,3.220311302328));
#22972=CARTESIAN_POINT('Ctrl Pts',(4.25585590634587,0.263669291018626,3.21356743282028));
#22973=CARTESIAN_POINT('Ctrl Pts',(4.24955975325296,0.365088513931847,3.20200373820754));
#22974=CARTESIAN_POINT('Ctrl Pts',(4.24326260798755,0.466523718883887,3.19043822134245));
#22975=CARTESIAN_POINT('Ctrl Pts',(4.23696546272215,0.567382358389521,3.17405142095642));
#22976=CARTESIAN_POINT('Ctrl Pts',(4.23066831745674,0.667189862659268,3.15293121549848));
#22977=CARTESIAN_POINT('Ctrl Pts',(4.22436580945623,0.767082364365909,3.13179302378445));
#22978=CARTESIAN_POINT('Ctrl Pts',(4.21806330145572,0.86592154302919,3.10591346756781));
#22979=CARTESIAN_POINT('Ctrl Pts',(4.21176079345521,0.963244981248796,3.07543113540183));
#22980=CARTESIAN_POINT('Ctrl Pts',(4.20791616452323,1.02261380812033,3.05683643371323));
#22981=CARTESIAN_POINT('Ctrl Pts',(4.20407153559125,1.08141888564317,3.03652993000679));
#22982=CARTESIAN_POINT('Ctrl Pts',(4.20022690665927,1.13955862823483,3.01455198915453));
#22983=CARTESIAN_POINT('Ctrl Pts',(4.19377635600178,1.2371059758296,2.9776772157179));
#22984=CARTESIAN_POINT('Ctrl Pts',(4.18732580534429,1.33291336564918,2.93604417137762));
#22985=CARTESIAN_POINT('Ctrl Pts',(4.18087525468681,1.42651379475993,2.88984012634949));
#22986=CARTESIAN_POINT('Ctrl Pts',(4.17442859288135,1.52005779485586,2.84366393641526));
#22987=CARTESIAN_POINT('Ctrl Pts',(4.16798193107589,1.61139714563366,2.79292240306838));
#22988=CARTESIAN_POINT('Ctrl Pts',(4.16153526927044,1.70008647398485,2.73785016819288));
#22989=CARTESIAN_POINT('Ctrl Pts',(4.15509160053378,1.78873462548057,2.68280350236269));
#22990=CARTESIAN_POINT('Ctrl Pts',(4.14864793179712,1.87473488450725,2.62343034099842));
#22991=CARTESIAN_POINT('Ctrl Pts',(4.14220426306046,1.95766836532562,2.56001018238274));
#22992=CARTESIAN_POINT('Ctrl Pts',(4.13576269432608,2.04057481798564,2.49661069250149));
#22993=CARTESIAN_POINT('Ctrl Pts',(4.12932112559171,2.12041618366918,2.42916706414711));
#22994=CARTESIAN_POINT('Ctrl Pts',(4.12287955685733,2.1968046271748,2.35800063454686));
#22995=CARTESIAN_POINT('Ctrl Pts',(4.11643824441589,2.27319003138686,2.28683703647009));
#22996=CARTESIAN_POINT('Ctrl Pts',(4.10999693197444,2.34612250647129,2.21195118690088));
#22997=CARTESIAN_POINT('Ctrl Pts',(4.103555619533,2.4152493307578,2.13370293920546));
#22998=CARTESIAN_POINT('Ctrl Pts',(4.09711486695258,2.48437014673239,2.05546149263079));
#22999=CARTESIAN_POINT('Ctrl Pts',(4.09067411437216,2.54968572303579,1.9738585168972));
#23000=CARTESIAN_POINT('Ctrl Pts',(4.08423336179173,2.61088248542984,1.88928828127835));
#23001=CARTESIAN_POINT('Ctrl Pts',(4.07779092924952,2.67209520996826,1.80469598693846));
#23002=CARTESIAN_POINT('Ctrl Pts',(4.07134849670731,2.72918675307052,1.71713519437524));
#23003=CARTESIAN_POINT('Ctrl Pts',(4.06490606416509,2.78188589731074,1.62703055190849));
#23004=CARTESIAN_POINT('Ctrl Pts',(4.06208259915809,2.8049818612477,1.58754122806902));
#23005=CARTESIAN_POINT('Ctrl Pts',(4.05925913415108,2.82723473678362,1.54756366161791));
#23006=CARTESIAN_POINT('Ctrl Pts',(4.05643566914408,2.84862442585767,1.5071351773836));
#23007=CARTESIAN_POINT('Ctrl Pts',(4.24126248314343,-2.84862442585767,1.50713517738358));
#23008=CARTESIAN_POINT('Ctrl Pts',(4.23481876049118,-2.79980879553496,1.59940121893556));
#23009=CARTESIAN_POINT('Ctrl Pts',(4.22837503783893,-2.74649436014097,1.68931672321789));
#23010=CARTESIAN_POINT('Ctrl Pts',(4.22193131518668,-2.6889328678291,1.77644521300501));
#23011=CARTESIAN_POINT('Ctrl Pts',(4.21548902163385,-2.63138414159976,1.8635543792922));
#23012=CARTESIAN_POINT('Ctrl Pts',(4.20904672808102,-2.56959044436887,1.94787744697516));
#23013=CARTESIAN_POINT('Ctrl Pts',(4.20260443452819,-2.50384730577855,2.0290062177937));
#23014=CARTESIAN_POINT('Ctrl Pts',(4.19616268405277,-2.43810970925386,2.11012814955677));
#23015=CARTESIAN_POINT('Ctrl Pts',(4.18972093357736,-2.36842357401578,2.1880560273807));
#23016=CARTESIAN_POINT('Ctrl Pts',(4.18327918310194,-2.29512500726732,2.26241436600729));
#23017=CARTESIAN_POINT('Ctrl Pts',(4.17683709017549,-2.22182254388083,2.33677665761064));
#23018=CARTESIAN_POINT('Ctrl Pts',(4.17039499724904,-2.14490753324225,2.40756876318795));
#23019=CARTESIAN_POINT('Ctrl Pts',(4.16395290432258,-2.06475300377837,2.47445197890123));
#23020=CARTESIAN_POINT('Ctrl Pts',(4.15750743506085,-1.98455646489775,2.54137024846487));
#23021=CARTESIAN_POINT('Ctrl Pts',(4.15106196579911,-1.90111730565429,2.60437529159052));
#23022=CARTESIAN_POINT('Ctrl Pts',(4.14461649653737,-1.81484181987328,2.663168551057));
#23023=CARTESIAN_POINT('Ctrl Pts',(4.13816950067629,-1.72854589987803,2.72197573561528));
#23024=CARTESIAN_POINT('Ctrl Pts',(4.13172250481521,-1.63941263144259,2.77656894057831));
#23025=CARTESIAN_POINT('Ctrl Pts',(4.12527550895413,-1.54787664770338,2.82669337672032));
#23026=CARTESIAN_POINT('Ctrl Pts',(4.11882374926244,-1.45627302596195,2.87685485093835));
#23027=CARTESIAN_POINT('Ctrl Pts',(4.11237198957076,-1.36226347780444,2.92254078344268));
#23028=CARTESIAN_POINT('Ctrl Pts',(4.10592022987908,-1.2663067134988,2.96354262156762));
#23029=CARTESIAN_POINT('Ctrl Pts',(4.10310390179547,-1.22441957835406,2.98144078171453));
#23030=CARTESIAN_POINT('Ctrl Pts',(4.10028757371185,-1.18216166644338,2.99844700132402));
#23031=CARTESIAN_POINT('Ctrl Pts',(4.09747124562824,-1.1395722534486,3.0145468385265));
#23032=CARTESIAN_POINT('Ctrl Pts',(4.09117032668804,-1.04428774432049,3.05056670771484));
#23033=CARTESIAN_POINT('Ctrl Pts',(4.08486940774784,-0.94721468089237,3.08209480971671));
#23034=CARTESIAN_POINT('Ctrl Pts',(4.07856848880764,-0.848804201550354,
3.10896268712419));
#23035=CARTESIAN_POINT('Ctrl Pts',(4.07227176894274,-0.750459305183979,
3.13581265916873));
#23036=CARTESIAN_POINT('Ctrl Pts',(4.06597504907784,-0.6507791607072,3.15800847802623));
#23037=CARTESIAN_POINT('Ctrl Pts',(4.05967832921294,-0.550230920981323,
3.1754312299428));
#23038=CARTESIAN_POINT('Ctrl Pts',(4.05338440237998,-0.449727281372719,
3.19284625366064));
#23039=CARTESIAN_POINT('Ctrl Pts',(4.04709047554701,-0.348356716342556,
3.20549235420444));
#23040=CARTESIAN_POINT('Ctrl Pts',(4.04079654871405,-0.246596769234935,
3.21330166587311));
#23041=CARTESIAN_POINT('Ctrl Pts',(4.03450401171771,-0.14485929294807,3.22110925307505));
#23042=CARTESIAN_POINT('Ctrl Pts',(4.02821147472137,-0.0427330144242478,
3.22408214721155));
#23043=CARTESIAN_POINT('Ctrl Pts',(4.02191893772504,0.0592998919896358,
3.22220438292018));
#23044=CARTESIAN_POINT('Ctrl Pts',(4.01562425890107,0.161367527940822,3.2203259794832));
#23045=CARTESIAN_POINT('Ctrl Pts',(4.0093295800771,0.263341317904613,3.21359362212927));
#23046=CARTESIAN_POINT('Ctrl Pts',(4.00303490125313,0.364739787469471,3.20204348033201));
#23047=CARTESIAN_POINT('Ctrl Pts',(3.99673922758709,0.466154282548244,3.19049151309341));
#23048=CARTESIAN_POINT('Ctrl Pts',(3.99044355392106,0.566992869424478,3.17412029923523));
#23049=CARTESIAN_POINT('Ctrl Pts',(3.98414788025502,0.666781168304401,3.15301767138952));
#23050=CARTESIAN_POINT('Ctrl Pts',(3.97784682745646,0.766654728033676,3.13189701309342));
#23051=CARTESIAN_POINT('Ctrl Pts',(3.9715457746579,0.8654758072472,3.10603695831234));
#23052=CARTESIAN_POINT('Ctrl Pts',(3.96524472185934,0.962782178547027,3.07557604997377));
#23053=CARTESIAN_POINT('Ctrl Pts',(3.96138981727725,1.02231298848977,3.05694045067268));
#23054=CARTESIAN_POINT('Ctrl Pts',(3.95753491269516,1.08127715485643,3.03658380806987));
#23055=CARTESIAN_POINT('Ctrl Pts',(3.95368000811307,1.13957225344858,3.0145468385265));
#23056=CARTESIAN_POINT('Ctrl Pts',(3.947228496954,1.23713406621913,2.97766609299998));
#23057=CARTESIAN_POINT('Ctrl Pts',(3.94077698579493,1.33295510131961,2.93602576269598));
#23058=CARTESIAN_POINT('Ctrl Pts',(3.93432547463586,1.42656825190966,2.88981324399059));
#23059=CARTESIAN_POINT('Ctrl Pts',(3.92787784149396,1.52012513143452,2.8436285037291));
#23060=CARTESIAN_POINT('Ctrl Pts',(3.92143020835205,1.6114764313792,2.79287721761468));
#23061=CARTESIAN_POINT('Ctrl Pts',(3.91498257521015,1.70017668345824,2.73779414995447));
#23062=CARTESIAN_POINT('Ctrl Pts',(3.90853792862088,1.7888358494573,2.68273659684773));
#23063=CARTESIAN_POINT('Ctrl Pts',(3.9020932820316,1.87484609299292,2.62335145979373));
#23064=CARTESIAN_POINT('Ctrl Pts',(3.89564863544233,1.95778843947618,2.55991835587649));
#23065=CARTESIAN_POINT('Ctrl Pts',(3.889206086644,2.04070378747302,2.4965059000102));
#23066=CARTESIAN_POINT('Ctrl Pts',(3.88276353784567,2.12055292816708,2.4290483334246));
#23067=CARTESIAN_POINT('Ctrl Pts',(3.87632098904734,2.19694794161334,2.35786710913506));
#23068=CARTESIAN_POINT('Ctrl Pts',(3.869878703417,2.2733398344434,2.28668879248663));
#23069=CARTESIAN_POINT('Ctrl Pts',(3.86343641778667,2.34627760067319,2.21178737573021));
#23070=CARTESIAN_POINT('Ctrl Pts',(3.85699413215633,2.41540843679194,2.13352282527615));
#23071=CARTESIAN_POINT('Ctrl Pts',(3.85055241257265,2.48453319878091,2.05526515147893));
#23072=CARTESIAN_POINT('Ctrl Pts',(3.84411069298898,2.54985144934752,1.97364521927884));
#23073=CARTESIAN_POINT('Ctrl Pts',(3.8376689734053,2.61104953277672,1.88905741042628));
#23074=CARTESIAN_POINT('Ctrl Pts',(3.83122559223455,2.67226340173385,1.80444778286399));
#23075=CARTESIAN_POINT('Ctrl Pts',(3.82478221106381,2.72935475925089,1.71686905696282));
#23076=CARTESIAN_POINT('Ctrl Pts',(3.81833882989306,2.78205230648587,1.62674599322594));
#23077=CARTESIAN_POINT('Ctrl Pts',(3.81552214346133,2.80508873136103,1.58734922247993));
#23078=CARTESIAN_POINT('Ctrl Pts',(3.8127054570296,2.82728608915286,1.54746660090595));
#23079=CARTESIAN_POINT('Ctrl Pts',(3.80988877059788,2.84862442585767,1.5071351773836));
#23080=CARTESIAN_POINT('Origin',(13.3346225254169,0.,0.));
#23081=CARTESIAN_POINT('Ctrl Pts',(4.86626248314343,2.84862442585767,-1.50713517738359));
#23082=CARTESIAN_POINT('Ctrl Pts',(4.85981933345969,2.79981313616544,-1.59939301474379));
#23083=CARTESIAN_POINT('Ctrl Pts',(4.85337618377595,2.74650376206013,-1.68930088118904));
#23084=CARTESIAN_POINT('Ctrl Pts',(4.84693303409221,2.68894797104939,-1.77642235166342));
#23085=CARTESIAN_POINT('Ctrl Pts',(4.84049132185755,2.63140502057819,-1.86352438557603));
#23086=CARTESIAN_POINT('Ctrl Pts',(4.83404960962288,2.56961775001987,-1.9478409463242));
#23087=CARTESIAN_POINT('Ctrl Pts',(4.82760789738821,2.50388161105083,-2.02896388344926));
#23088=CARTESIAN_POINT('Ctrl Pts',(4.82116673398445,2.43815107277048,-2.11007990893753));
#23089=CARTESIAN_POINT('Ctrl Pts',(4.81472557058069,2.36847257578656,-2.18800255924028));
#23090=CARTESIAN_POINT('Ctrl Pts',(4.80828440717693,2.29518215168749,-2.26235639391215));
#23091=CARTESIAN_POINT('Ctrl Pts',(4.80184290448635,2.22188786703192,-2.33671414515543));
#23092=CARTESIAN_POINT('Ctrl Pts',(4.79540140179577,2.14498154315761,-2.4075024373787));
#23093=CARTESIAN_POINT('Ctrl Pts',(4.78895989910519,2.0648361346245,-2.47438260979359));
#23094=CARTESIAN_POINT('Ctrl Pts',(4.78251501843759,1.98464869717969,-2.54129785472121));
#23095=CARTESIAN_POINT('Ctrl Pts',(4.77607013776999,1.90121907212231,-2.60430064161492));
#23096=CARTESIAN_POINT('Ctrl Pts',(4.76962525710239,1.8149534807021,-2.66309245528339));
#23097=CARTESIAN_POINT('Ctrl Pts',(4.76317884768156,1.72866742671495,-2.72189821462132));
#23098=CARTESIAN_POINT('Ctrl Pts',(4.75673243826072,1.63954438272681,-2.77649080212196));
#23099=CARTESIAN_POINT('Ctrl Pts',(4.75028602883989,1.54801890922746,-2.82661547069534));
#23100=CARTESIAN_POINT('Ctrl Pts',(4.74383484637411,1.45642566851539,-2.8767772525329));
#23101=CARTESIAN_POINT('Ctrl Pts',(4.73738366390833,1.36242678053088,-2.92246433038377));
#23102=CARTESIAN_POINT('Ctrl Pts',(4.73093248144255,1.26648088252647,-2.96346819397391));
#23103=CARTESIAN_POINT('Ctrl Pts',(4.72811206950445,1.22453400572065,-2.9813947968861));
#23104=CARTESIAN_POINT('Ctrl Pts',(4.72529165756634,1.18221524872853,-2.99842687834116));
#23105=CARTESIAN_POINT('Ctrl Pts',(4.72247124562824,1.13956406305674,-3.01454993468173));
#23106=CARTESIAN_POINT('Ctrl Pts',(4.71616945312009,1.04426630931427,-3.05057451473779));
#23107=CARTESIAN_POINT('Ctrl Pts',(4.70986766061195,0.947179779202421,-3.08210598637527));
#23108=CARTESIAN_POINT('Ctrl Pts',(4.70356586810381,0.84875574859297,-3.10897591527023));
#23109=CARTESIAN_POINT('Ctrl Pts',(4.69726826800526,0.750397196789678,-3.13582796833899));
#23110=CARTESIAN_POINT('Ctrl Pts',(4.69097066790671,0.650703309207103,-3.15802454125043));
#23111=CARTESIAN_POINT('Ctrl Pts',(4.68467306780816,0.550141367953137,-3.17544674617079));
#23112=CARTESIAN_POINT('Ctrl Pts',(4.67837825616033,0.449623953505189,-3.19286123688904));
#23113=CARTESIAN_POINT('Ctrl Pts',(4.67208344451251,0.348239653662265,-3.2055054971021));
#23114=CARTESIAN_POINT('Ctrl Pts',(4.66578863286469,0.246466134457317,-3.21331168844008));
#23115=CARTESIAN_POINT('Ctrl Pts',(4.65949520855386,0.14471504549758,-3.22111615934247));
#23116=CARTESIAN_POINT('Ctrl Pts',(4.65320178424304,0.04257531645346,-3.22408465366294));
#23117=CARTESIAN_POINT('Ctrl Pts',(4.64690835993221,-0.0594707603238784,
-3.22220123380997));
#23118=CARTESIAN_POINT('Ctrl Pts',(4.64061279625238,-0.161551526358372,
-3.22031717371254));
#23119=CARTESIAN_POINT('Ctrl Pts',(4.63431723257254,-0.263538166304509,
-3.21357790737857));
#23120=CARTESIAN_POINT('Ctrl Pts',(4.62802166889271,-0.364949091061416,
-3.20201963195628));
#23121=CARTESIAN_POINT('Ctrl Pts',(4.62172511196881,-0.46637601530677,-3.19045953299778));
#23122=CARTESIAN_POINT('Ctrl Pts',(4.61542855504492,-0.567226636915087,
-3.174078965025));
#23123=CARTESIAN_POINT('Ctrl Pts',(4.60913199812103,-0.667026462081897,
-3.15296578817191));
#23124=CARTESIAN_POINT('Ctrl Pts',(4.60283007189777,-0.766911390130261,
-3.13183460735753));
#23125=CARTESIAN_POINT('Ctrl Pts',(4.59652814567451,-0.865743332042191,
-3.1059628489963));
#23126=CARTESIAN_POINT('Ctrl Pts',(4.59022621945125,-0.963059946406137,
-3.07548908340254));
#23127=CARTESIAN_POINT('Ctrl Pts',(4.58637748233852,-1.0224935310148,-3.05687802569571));
#23128=CARTESIAN_POINT('Ctrl Pts',(4.58252874522579,-1.08136220999437,-3.03655147441081));
#23129=CARTESIAN_POINT('Ctrl Pts',(4.57868000811306,-1.13956406305672,-3.01454993468173));
#23130=CARTESIAN_POINT('Ctrl Pts',(4.57222907503224,-1.23711716899467,-2.97767278347336));
#23131=CARTESIAN_POINT('Ctrl Pts',(4.56577814195141,-1.33292999080922,-2.93603683833042));
#23132=CARTESIAN_POINT('Ctrl Pts',(4.55932720887058,-1.42653548420085,-2.88982941967443));
#23133=CARTESIAN_POINT('Ctrl Pts',(4.55288016033801,-1.52008461131938,-2.84364982566724));
#23134=CARTESIAN_POINT('Ctrl Pts',(4.54643311180544,-1.61142871884073,-2.79290440957343));
#23135=CARTESIAN_POINT('Ctrl Pts',(4.53998606327287,-1.7001223957646,-2.73782786199565));
#23136=CARTESIAN_POINT('Ctrl Pts',(4.5335420052227,-1.78877493186577,-2.68277686183632));
#23137=CARTESIAN_POINT('Ctrl Pts',(4.52709794717254,-1.87477916552009,-2.62339893285564));
#23138=CARTESIAN_POINT('Ctrl Pts',(4.52065388912237,-1.9577161756141,-2.55997362061387));
#23139=CARTESIAN_POINT('Ctrl Pts',(4.51421193019997,-2.04062616928784,-2.49656896892991));
#23140=CARTESIAN_POINT('Ctrl Pts',(4.50776997127757,-2.1204706300486,-2.42911979172178));
#23141=CARTESIAN_POINT('Ctrl Pts',(4.50132801235517,-2.19686168895409,-2.35794747229573));
#23142=CARTESIAN_POINT('Ctrl Pts',(4.49488631246818,-2.27324967612483,-2.28677801475546));
#23143=CARTESIAN_POINT('Ctrl Pts',(4.48844461258119,-2.34618425752059,-2.21188596787905));
#23144=CARTESIAN_POINT('Ctrl Pts',(4.48200291269419,-2.41531267888492,-2.13363123002026));
#23145=CARTESIAN_POINT('Ctrl Pts',(4.47556177513205,-2.48443506571956,-2.05538332336822));
#23146=CARTESIAN_POINT('Ctrl Pts',(4.4691206375699,-2.54975170666112,-1.97377359722138));
#23147=CARTESIAN_POINT('Ctrl Pts',(4.46267950000776,-2.61094899502869,-1.88919636561653));
#23148=CARTESIAN_POINT('Ctrl Pts',(4.45623668979986,-2.67216217521413,-1.80459717084963));
#23149=CARTESIAN_POINT('Ctrl Pts',(4.44979387959195,-2.72925364454466,-1.71702923891643));
#23150=CARTESIAN_POINT('Ctrl Pts',(4.44335106938405,-2.78195215317476,-1.62691726278454));
#23151=CARTESIAN_POINT('Ctrl Pts',(4.44053030312199,-2.80502441052948,-1.58746478570115));
#23152=CARTESIAN_POINT('Ctrl Pts',(4.43770953685994,-2.82725518163247,-1.5475250189688));
#23153=CARTESIAN_POINT('Ctrl Pts',(4.43488877059788,-2.84862442585766,-1.50713517738361));
#23154=CARTESIAN_POINT('Ctrl Pts',(5.11280938168962,2.84862442585767,-1.50713517738359));
#23155=CARTESIAN_POINT('Ctrl Pts',(5.10636711383503,2.79981981662761,-1.59938038805443));
#23156=CARTESIAN_POINT('Ctrl Pts',(5.09992484598043,2.74651823180318,-1.6892764997169));
#23157=CARTESIAN_POINT('Ctrl Pts',(5.09348257812584,2.68897121470972,-1.77638716752923));
#23158=CARTESIAN_POINT('Ctrl Pts',(5.08704176057363,2.63143715277091,-1.86347822473044));
#23159=CARTESIAN_POINT('Ctrl Pts',(5.08060094302142,2.56965977216091,-1.94778477152975));
#23160=CARTESIAN_POINT('Ctrl Pts',(5.07416012546921,2.50393440450652,-2.02889873094459));
#23161=CARTESIAN_POINT('Ctrl Pts',(5.06771986561689,2.43821472790447,-2.11000566683405));
#23162=CARTESIAN_POINT('Ctrl Pts',(5.06127960576456,2.36854798484811,-2.18792027227159));
#23163=CARTESIAN_POINT('Ctrl Pts',(5.05483934591224,2.29527009050459,-2.26226717567467));
#23164=CARTESIAN_POINT('Ctrl Pts',(5.04839875166834,2.2219883914217,-2.33661793932228));
#23165=CARTESIAN_POINT('Ctrl Pts',(5.04195815742445,2.1450954345748,-2.40740036286648));
#23166=CARTESIAN_POINT('Ctrl Pts',(5.03551756318055,2.06496406080377,-2.47427585165616));
#23167=CARTESIAN_POINT('Ctrl Pts',(5.02907358849095,1.98479062883933,-2.54118644108257));
#23168=CARTESIAN_POINT('Ctrl Pts',(5.02262961380134,1.90137567487522,-2.60418575505825));
#23169=CARTESIAN_POINT('Ctrl Pts',(5.01618563911174,1.8151253084368,-2.66297534295236));
#23170=CARTESIAN_POINT('Ctrl Pts',(5.00974013239813,1.72885443638833,-2.7217789077884));
#23171=CARTESIAN_POINT('Ctrl Pts',(5.00329462568452,1.63974712559499,-2.77637054387109));
#23172=CARTESIAN_POINT('Ctrl Pts',(4.99684911897091,1.54823782472648,-2.8264955688248));
#23173=CARTESIAN_POINT('Ctrl Pts',(4.99039882510423,1.4566605588321,-2.87665782221961));
#23174=CARTESIAN_POINT('Ctrl Pts',(4.98394853123755,1.36267807492272,-2.92234666080682));
#23175=CARTESIAN_POINT('Ctrl Pts',(4.97749823737087,1.26674889787392,-2.96335363941518));
#23176=CARTESIAN_POINT('Ctrl Pts',(4.97467153963873,1.22471007099033,-2.98132403515682));
#23177=CARTESIAN_POINT('Ctrl Pts',(4.97184484190659,1.18229766210062,-2.99839592961301));
#23178=CARTESIAN_POINT('Ctrl Pts',(4.96901814417446,1.13955139439377,-3.01455472367566));
#23179=CARTESIAN_POINT('Ctrl Pts',(4.96271499237138,1.04423302649469,-3.05058663850462));
#23180=CARTESIAN_POINT('Ctrl Pts',(4.95641184056829,0.947125536289407,-3.08212335702997));
#23181=CARTESIAN_POINT('Ctrl Pts',(4.95010868876521,0.848680413718823,-3.10899648083912));
#23182=CARTESIAN_POINT('Ctrl Pts',(4.94380971895555,0.750300607178534,-3.1358517749608));
#23183=CARTESIAN_POINT('Ctrl Pts',(4.93751074914588,0.65058532817276,-3.15804952315385));
#23184=CARTESIAN_POINT('Ctrl Pts',(4.93121177933621,0.550002060058652,-3.17547087790634));
#23185=CARTESIAN_POINT('Ctrl Pts',(4.92491559082192,0.449463204251157,-3.19288454030041));
#23186=CARTESIAN_POINT('Ctrl Pts',(4.91861940230763,0.348057525191484,-3.20552593692252));
#23187=CARTESIAN_POINT('Ctrl Pts',(4.91232321379334,0.246262879960412,-3.21332727191825));
#23188=CARTESIAN_POINT('Ctrl Pts',(4.90602840871693,0.144490601684816,-3.22112689275592));
#23189=CARTESIAN_POINT('Ctrl Pts',(4.89973360364052,0.0423299356387917,
-3.22408853877205));
#23190=CARTESIAN_POINT('Ctrl Pts',(4.89343879856411,-0.0597366420634672,
-3.22219631557343));
#23191=CARTESIAN_POINT('Ctrl Pts',(4.88714185796157,-0.161837846071059,
-3.22030345043403));
#23192=CARTESIAN_POINT('Ctrl Pts',(4.88084491735904,-0.263844488001992,
-3.21355342937545));
#23193=CARTESIAN_POINT('Ctrl Pts',(4.87454797675651,-0.365274800146589,
-3.2019824925939));
#23194=CARTESIAN_POINT('Ctrl Pts',(4.86825004542209,-0.46672107087347,-3.19040973529399));
#23195=CARTESIAN_POINT('Ctrl Pts',(4.86195211408767,-0.567590424925492,
-3.17401460588662));
#23196=CARTESIAN_POINT('Ctrl Pts',(4.85565418275325,-0.667408190937708,
-3.15288500728607));
#23197=CARTESIAN_POINT('Ctrl Pts',(4.84935089747216,-0.767310813225424,
-3.13173744616129));
#23198=CARTESIAN_POINT('Ctrl Pts',(4.84304761219107,-0.866159662195225,
-3.10584746878142));
#23199=CARTESIAN_POINT('Ctrl Pts',(4.83674432690997,-0.963492218863993,
-3.07535368806395));
#23200=CARTESIAN_POINT('Ctrl Pts',(4.8329051868264,-1.02277453008417,-3.05678085014986));
#23201=CARTESIAN_POINT('Ctrl Pts',(4.82906604674283,-1.08149463511915,-3.03650113601502));
#23202=CARTESIAN_POINT('Ctrl Pts',(4.82522690665926,-1.13955139439361,-3.01455472367572));
#23203=CARTESIAN_POINT('Ctrl Pts',(4.81877686346817,-1.23709110294912,-2.97768310544958));
#23204=CARTESIAN_POINT('Ctrl Pts',(4.81232682027708,-1.33289128658037,-2.93605391017899));
#23205=CARTESIAN_POINT('Ctrl Pts',(4.80587677708598,-1.42648499723591,-2.88985434151289));
#23206=CARTESIAN_POINT('Ctrl Pts',(4.79943062843622,-1.52002219593272,-2.84368266818397));
#23207=CARTESIAN_POINT('Ctrl Pts',(4.79298447978646,-1.61135523643265,-2.79294628646449));
#23208=CARTESIAN_POINT('Ctrl Pts',(4.7865383311367,-1.70003879590331,-2.73787977364303));
#23209=CARTESIAN_POINT('Ctrl Pts',(4.78009517897046,-1.78868113094077,-2.68283885841591));
#23210=CARTESIAN_POINT('Ctrl Pts',(4.77365202680422,-1.87467611728968,-2.6234720224791));
#23211=CARTESIAN_POINT('Ctrl Pts',(4.76720887463797,-1.95760491614971,-2.56005870142981));
#23212=CARTESIAN_POINT('Ctrl Pts',(4.76076782362139,-2.0405066714427,-2.49666605983594));
#23213=CARTESIAN_POINT('Ctrl Pts',(4.75432677260481,-2.12034393124181,-2.42922979327325));
#23214=CARTESIAN_POINT('Ctrl Pts',(4.74788572158823,-2.19672890512053,-2.35807117787143));
#23215=CARTESIAN_POINT('Ctrl Pts',(4.74144492321345,-2.27311088289856,-2.28691535357323));
#23216=CARTESIAN_POINT('Ctrl Pts',(4.73500412483867,-2.34604056377377,-2.21203772602462));
#23217=CARTESIAN_POINT('Ctrl Pts',(4.72856332646389,-2.4151652693211,-2.13379808894027));
#23218=CARTESIAN_POINT('Ctrl Pts',(4.72212308467781,-2.48428400138074,-2.05556521302048));
#23219=CARTESIAN_POINT('Ctrl Pts',(4.71568284289172,-2.54959816524026,-1.97397119318511));
#23220=CARTESIAN_POINT('Ctrl Pts',(4.70924260110564,-2.61079422971956,-1.88941023935064));
#23221=CARTESIAN_POINT('Ctrl Pts',(4.70280066964823,-2.6720063496885,-1.80482709997974));
#23222=CARTESIAN_POINT('Ctrl Pts',(4.69635873819083,-2.72909799048163,-1.71727577947338));
#23223=CARTESIAN_POINT('Ctrl Pts',(4.68991680673342,-2.7817979777028,-1.62718086694399));
#23224=CARTESIAN_POINT('Ctrl Pts',(4.68708976087031,-2.8049254018061,-1.58764265523871));
#23225=CARTESIAN_POINT('Ctrl Pts',(4.6842627150072,-2.82720760933608,-1.54761493499459));
#23226=CARTESIAN_POINT('Ctrl Pts',(4.68143566914408,-2.84862442585766,-1.50713517738361));
#23227=CARTESIAN_POINT('Origin',(13.3346225254169,0.,0.));
#23228=CARTESIAN_POINT('Ctrl Pts',(5.73780938168963,-2.84862442585767,1.50713517738358));
#23229=CARTESIAN_POINT('Ctrl Pts',(5.73136758080448,-2.79982335424228,1.59937370163659));
#23230=CARTESIAN_POINT('Ctrl Pts',(5.72492577991932,-2.74652589403969,1.68926358874148));
#23231=CARTESIAN_POINT('Ctrl Pts',(5.71848397903417,-2.68898352277793,1.77636853629218));
#23232=CARTESIAN_POINT('Ctrl Pts',(5.71204363526109,-2.63145416739255,1.8634537810186));
#23233=CARTESIAN_POINT('Ctrl Pts',(5.70560329148801,-2.5696820234343,1.9477550252753));
#23234=CARTESIAN_POINT('Ctrl Pts',(5.69916294771493,-2.5039623589255,2.02886423093913));
#23235=CARTESIAN_POINT('Ctrl Pts',(5.69272316634707,-2.43824843340877,2.10996635371399));
#23236=CARTESIAN_POINT('Ctrl Pts',(5.6862833849792,-2.36858791370451,2.18787669933437));
#23237=CARTESIAN_POINT('Ctrl Pts',(5.67984360361133,-2.29531665330212,2.26221993262679));
#23238=CARTESIAN_POINT('Ctrl Pts',(5.6734034904585,-2.22204161787986,2.33656699616836));
#23239=CARTESIAN_POINT('Ctrl Pts',(5.66696337730567,-2.14515573827782,2.40734631214546));
#23240=CARTESIAN_POINT('Ctrl Pts',(5.66052326415283,-2.06503179509463,2.47421932086633));
#23241=CARTESIAN_POINT('Ctrl Pts',(5.65407976927837,-1.98486577860227,2.54112744479321));
#23242=CARTESIAN_POINT('Ctrl Pts',(5.64763627440391,-1.90145859236094,2.60412491949775));
#23243=CARTESIAN_POINT('Ctrl Pts',(5.64119277952944,-1.81521628671604,2.66291332846956));
#23244=CARTESIAN_POINT('Ctrl Pts',(5.63474775092228,-1.72895345298092,2.72171573073335));
#23245=CARTESIAN_POINT('Ctrl Pts',(5.62830272231512,-1.6398544721981,2.77630686247375));
#23246=CARTESIAN_POINT('Ctrl Pts',(5.62185769370796,-1.54835373381425,2.82643207551207));
#23247=CARTESIAN_POINT('Ctrl Pts',(5.61540787051526,-1.45678492620307,2.8765945776978));
#23248=CARTESIAN_POINT('Ctrl Pts',(5.60895804732255,-1.36281112768951,2.92228434769856));
#23249=CARTESIAN_POINT('Ctrl Pts',(5.60250822412985,-1.26689080363705,2.96329297474277));
#23250=CARTESIAN_POINT('Ctrl Pts',(5.59967819747804,-1.22480328194728,2.98128656991919));
#23251=CARTESIAN_POINT('Ctrl Pts',(5.59684817082624,-1.18234127527403,2.99837955251588));
#23252=CARTESIAN_POINT('Ctrl Pts',(5.59401814417444,-1.13954465120738,3.01455727270269));
#23253=CARTESIAN_POINT('Ctrl Pts',(5.58771426446053,-1.04421524146304,3.05059311782018));
#23254=CARTESIAN_POINT('Ctrl Pts',(5.58141038474663,-0.947096523955763,
3.08213264808556));
#23255=CARTESIAN_POINT('Ctrl Pts',(5.57510650503273,-0.848640103333476,
3.10900748431298));
#23256=CARTESIAN_POINT('Ctrl Pts',(5.56880680171199,-0.75024891122765,3.13586451565083));
#23257=CARTESIAN_POINT('Ctrl Pts',(5.56250709839125,-0.650522173317262,
3.15806289431417));
#23258=CARTESIAN_POINT('Ctrl Pts',(5.5562073950705,-0.549927480801481,3.17548379437832));
#23259=CARTESIAN_POINT('Ctrl Pts',(5.54991046919983,-0.449377139062347,
3.19289701381412));
#23260=CARTESIAN_POINT('Ctrl Pts',(5.54361354332915,-0.347960007274539,
3.20553687704002));
#23261=CARTESIAN_POINT('Ctrl Pts',(5.53731661745847,-0.246154044899148,
3.21333561096251));
#23262=CARTESIAN_POINT('Ctrl Pts',(5.53102107293278,-0.144370415509591,
3.22113263409115));
#23263=CARTESIAN_POINT('Ctrl Pts',(5.52472552840709,-0.0421985334635265,
3.2240906117739));
#23264=CARTESIAN_POINT('Ctrl Pts',(5.5184299838814,0.0598790266433576,3.2221936727435));
#23265=CARTESIAN_POINT('Ctrl Pts',(5.51213230589621,0.161991179205344,3.22029609087076));
#23266=CARTESIAN_POINT('Ctrl Pts',(5.50583462791101,0.264008536143621,3.21354030846408));
#23267=CARTESIAN_POINT('Ctrl Pts',(5.49953694992581,0.365449234025181,3.20196258876496));
#23268=CARTESIAN_POINT('Ctrl Pts',(5.49323828256693,0.466905868376912,3.19038305019049));
#23269=CARTESIAN_POINT('Ctrl Pts',(5.48693961520804,0.567785257085751,3.1739801198557));
#23270=CARTESIAN_POINT('Ctrl Pts',(5.48064094784916,0.667612633620952,3.15284172357727));
#23271=CARTESIAN_POINT('Ctrl Pts',(5.4743369347914,0.767524733965719,3.1316853870752));
#23272=CARTESIAN_POINT('Ctrl Pts',(5.46803292173365,0.866382639234982,3.10578564917918));
#23273=CARTESIAN_POINT('Ctrl Pts',(5.46172890867589,0.963723735270517,3.07528114561519));
#23274=CARTESIAN_POINT('Ctrl Pts',(5.45789490800369,1.02292504469274,3.05672879077419));
#23275=CARTESIAN_POINT('Ctrl Pts',(5.45406090733147,1.08156559106839,3.03647416526322));
#23276=CARTESIAN_POINT('Ctrl Pts',(5.45022690665927,1.13954465120736,3.01455727270269));
#23277=CARTESIAN_POINT('Ctrl Pts',(5.44377733481477,1.23707726682557,2.97768858506739));
#23278=CARTESIAN_POINT('Ctrl Pts',(5.43732776297028,1.3328707593346,2.93606296465374));
#23279=CARTESIAN_POINT('Ctrl Pts',(5.43087819112579,1.42645823164935,2.88986755334216));
#23280=CARTESIAN_POINT('Ctrl Pts',(5.4244325190837,1.51998911530078,2.84370007457874));
#23281=CARTESIAN_POINT('Ctrl Pts',(5.41798684704161,1.61131629666718,2.79296847706825));
#23282=CARTESIAN_POINT('Ctrl Pts',(5.41154117499952,1.6999944996087,2.73790727815976));
#23283=CARTESIAN_POINT('Ctrl Pts',(5.40509850259378,1.78863143418289,2.68287170320063));
#23284=CARTESIAN_POINT('Ctrl Pts',(5.39865583018805,1.87462152487066,2.62351074129486));
#23285=CARTESIAN_POINT('Ctrl Pts',(5.39221315778232,1.95754597646872,2.56010376987167));
#23286=CARTESIAN_POINT('Ctrl Pts',(5.38577258757756,2.04044337037202,2.4967174877198));
#23287=CARTESIAN_POINT('Ctrl Pts',(5.37933201737281,2.12027681787577,2.42928805744418));
#23288=CARTESIAN_POINT('Ctrl Pts',(5.37289144716806,2.19665857014442,2.3581366984785));
#23289=CARTESIAN_POINT('Ctrl Pts',(5.36645112620017,2.27303736659577,2.28698809292462));
#23290=CARTESIAN_POINT('Ctrl Pts',(5.36001080523229,2.34596445307008,2.21211810038558));
#23291=CARTESIAN_POINT('Ctrl Pts',(5.35357048426441,2.41508719131533,2.13388645922051));
#23292=CARTESIAN_POINT('Ctrl Pts',(5.34713071684206,2.48420398846185,2.05566154206429));
#23293=CARTESIAN_POINT('Ctrl Pts',(5.3406909494197,2.5495168407891,1.97407583878954));
#23294=CARTESIAN_POINT('Ctrl Pts',(5.33425118199735,2.61071225711959,1.88952350422681));
#23295=CARTESIAN_POINT('Ctrl Pts',(5.32780971588266,2.6719238156766,1.80494886631164));
#23296=CARTESIAN_POINT('Ctrl Pts',(5.32136824976798,2.72901554704453,1.71740634179815));
#23297=CARTESIAN_POINT('Ctrl Pts',(5.31492678365329,2.78171631680616,1.62732046484839));
#23298=CARTESIAN_POINT('Ctrl Pts',(5.31209641215022,2.80487296379731,1.58773685229682));
#23299=CARTESIAN_POINT('Ctrl Pts',(5.30926604064715,2.82718241532643,1.54766255399543));
#23300=CARTESIAN_POINT('Ctrl Pts',(5.30643566914408,2.84862442585767,1.5071351773836));
#23301=CARTESIAN_POINT('Ctrl Pts',(5.49126248314343,-2.84862442585767,1.50713517738358));
#23302=CARTESIAN_POINT('Ctrl Pts',(5.48481986387308,-2.79981715441166,1.59938541988801));
#23303=CARTESIAN_POINT('Ctrl Pts',(5.47837724460274,-2.74651246554549,1.68928621588219));
#23304=CARTESIAN_POINT('Ctrl Pts',(5.47193462533239,-2.68896195208233,1.77640118857019));
#23305=CARTESIAN_POINT('Ctrl Pts',(5.46549345124158,-2.63142434809293,1.86349662001718));
#23306=CARTESIAN_POINT('Ctrl Pts',(5.45905227715078,-2.56964302641709,1.94780715736535));
#23307=CARTESIAN_POINT('Ctrl Pts',(5.45261110305997,-2.50391336653128,2.02892469436546));
#23308=CARTESIAN_POINT('Ctrl Pts',(5.44617048313234,-2.43818936166382,2.11003525245893));
#23309=CARTESIAN_POINT('Ctrl Pts',(5.43972986320472,-2.36851793483692,2.18795306374967));
#23310=CARTESIAN_POINT('Ctrl Pts',(5.43328924327709,-2.29523504761997,2.26230272922899));
#23311=CARTESIAN_POINT('Ctrl Pts',(5.42684828700312,-2.22194833337513,2.33665627744621));
#23312=CARTESIAN_POINT('Ctrl Pts',(5.42040733072914,-2.14505005001677,2.40744103965874));
#23313=CARTESIAN_POINT('Ctrl Pts',(5.41396637445516,-2.06491308370881,2.4743183948773));
#23314=CARTESIAN_POINT('Ctrl Pts',(5.40752203871037,-1.98473407076575,2.54123083961673));
#23315=CARTESIAN_POINT('Ctrl Pts',(5.40107770296558,-1.90131327063422,2.60423153763966));
#23316=CARTESIAN_POINT('Ctrl Pts',(5.3946333672208,-1.81505683736707,2.66302201260655));
#23317=CARTESIAN_POINT('Ctrl Pts',(5.38818750074876,-1.72877991555328,2.72182645211317));
#23318=CARTESIAN_POINT('Ctrl Pts',(5.38174163427671,-1.6396663353765,2.77641846750094));
#23319=CARTESIAN_POINT('Ctrl Pts',(5.37529576780467,-1.54815059006993,2.82654335062566));
#23320=CARTESIAN_POINT('Ctrl Pts',(5.36884511979071,-1.45656695840953,2.87670541637441));
#23321=CARTESIAN_POINT('Ctrl Pts',(5.36239447177675,-1.36257793772757,2.9223935535854));
#23322=CARTESIAN_POINT('Ctrl Pts',(5.3559438237628,-1.26664209768339,2.96339929116483));
#23323=CARTESIAN_POINT('Ctrl Pts',(5.35311963105128,-1.22463991439267,2.98135223247424));
#23324=CARTESIAN_POINT('Ctrl Pts',(5.35029543833976,-1.18226482780987,2.99840825960803));
#23325=CARTESIAN_POINT('Ctrl Pts',(5.34747124562824,-1.13955645269919,3.01455281154795));
#23326=CARTESIAN_POINT('Ctrl Pts',(5.34116863780042,-1.04424633516078,3.05058179038433));
#23327=CARTESIAN_POINT('Ctrl Pts',(5.3348660299726,-0.947147233815046,3.08211640860091));
#23328=CARTESIAN_POINT('Ctrl Pts',(5.32856342214479,-0.84871055291417,3.10898825341495));
#23329=CARTESIAN_POINT('Ctrl Pts',(5.32226500048531,-0.750339253285435,
3.13584225005102));
#23330=CARTESIAN_POINT('Ctrl Pts',(5.31596657882584,-0.650632535932309,
3.15803952760407));
#23331=CARTESIAN_POINT('Ctrl Pts',(5.30966815716637,-0.550057803653538,
3.17546122242736));
#23332=CARTESIAN_POINT('Ctrl Pts',(5.30337251966971,-0.44952752956525,3.19287521614113));
#23333=CARTESIAN_POINT('Ctrl Pts',(5.29707688217306,-0.348130407377017,
3.20551775872895));
#23334=CARTESIAN_POINT('Ctrl Pts',(5.2907812446764,-0.246344217693348,3.21332103732401));
#23335=CARTESIAN_POINT('Ctrl Pts',(5.28448699217943,-0.144580420315566,
3.22112259924806));
#23336=CARTESIAN_POINT('Ctrl Pts',(5.27819273968245,-0.0424281341942792,
3.22408698618299));
#23337=CARTESIAN_POINT('Ctrl Pts',(5.27189848718548,0.0596302381179428,
3.22219828645011));
#23338=CARTESIAN_POINT('Ctrl Pts',(5.26560209762197,0.161723261968531,3.22030894545331));
#23339=CARTESIAN_POINT('Ctrl Pts',(5.25930570805847,0.26372189824142,3.21356322893573));
#23340=CARTESIAN_POINT('Ctrl Pts',(5.25300931849496,0.365144450726462,3.20199735986832));
#23341=CARTESIAN_POINT('Ctrl Pts',(5.24671193719046,0.466582978224168,3.19042966906698));
#23342=CARTESIAN_POINT('Ctrl Pts',(5.24041455588597,0.567444834820857,3.17404036790822));
#23343=CARTESIAN_POINT('Ctrl Pts',(5.23411717458147,0.667255420232703,3.15291734218804));
#23344=CARTESIAN_POINT('Ctrl Pts',(5.22781443317866,0.76715096072735,3.13177633732875));
#23345=CARTESIAN_POINT('Ctrl Pts',(5.22151169177585,0.865993042988278,3.10589365218794));
#23346=CARTESIAN_POINT('Ctrl Pts',(5.21520895037304,0.963319219118907,3.07540788263543));
#23347=CARTESIAN_POINT('Ctrl Pts',(5.21136596961972,1.02266206658176,3.05681974484695));
#23348=CARTESIAN_POINT('Ctrl Pts',(5.20752298886639,1.08144162827987,3.03652128491847));
#23349=CARTESIAN_POINT('Ctrl Pts',(5.20368000811307,1.13955645269916,3.01455281154796));
#23350=CARTESIAN_POINT('Ctrl Pts',(5.19722961026351,1.23710149976634,2.97767898821057));
#23351=CARTESIAN_POINT('Ctrl Pts',(5.19077921241396,1.33290671942348,2.93604710292728));
#23352=CARTESIAN_POINT('Ctrl Pts',(5.18432881456441,1.42650512526415,2.88984440586256));
#23353=CARTESIAN_POINT('Ctrl Pts',(5.17788230728269,1.52004707707577,2.84366957602888));
#23354=CARTESIAN_POINT('Ctrl Pts',(5.17143580000098,1.61138452748375,2.79292959402038));
#23355=CARTESIAN_POINT('Ctrl Pts',(5.16498929271926,1.70007211851932,2.73785908226359));
#23356=CARTESIAN_POINT('Ctrl Pts',(5.15854577953673,1.78871851834361,2.68281414816721));
#23357=CARTESIAN_POINT('Ctrl Pts',(5.15210226635419,1.87471718947248,2.62344289164424));
#23358=CARTESIAN_POINT('Ctrl Pts',(5.14565875317165,1.95764926030105,2.56002479209533));
#23359=CARTESIAN_POINT('Ctrl Pts',(5.13921734033849,2.04055429831095,2.49662736452492));
#23360=CARTESIAN_POINT('Ctrl Pts',(5.13277592750534,2.1203944274837,2.42918595312001));
#23361=CARTESIAN_POINT('Ctrl Pts',(5.12633451467218,2.19678182610023,2.35802187670423));
#23362=CARTESIAN_POINT('Ctrl Pts',(5.11989335703403,2.27316619841126,2.28686061965709));
#23363=CARTESIAN_POINT('Ctrl Pts',(5.11345219939589,2.34609783200353,2.21197724610014));
#23364=CARTESIAN_POINT('Ctrl Pts',(5.10701104175774,2.41522401822815,2.13373159143175));
#23365=CARTESIAN_POINT('Ctrl Pts',(5.10057044299562,2.48434420662283,2.05549272585669));
#23366=CARTESIAN_POINT('Ctrl Pts',(5.0941298442335,2.54965935757275,1.97389244712996));
#23367=CARTESIAN_POINT('Ctrl Pts',(5.08768924547138,2.61085590980442,1.88932500664637));
#23368=CARTESIAN_POINT('Ctrl Pts',(5.08124696382397,2.67206845228505,1.80473546925737));
#23369=CARTESIAN_POINT('Ctrl Pts',(5.07480468217656,2.72916002482629,1.71717752912428));
#23370=CARTESIAN_POINT('Ctrl Pts',(5.06836240052915,2.78185942295809,1.62707581673359));
#23371=CARTESIAN_POINT('Ctrl Pts',(5.06553785721873,2.804964859914,1.58757177097474));
#23372=CARTESIAN_POINT('Ctrl Pts',(5.0627133139083,2.82722656789367,1.54757910157298));
#23373=CARTESIAN_POINT('Ctrl Pts',(5.05988877059788,2.84862442585765,1.50713517738362));
#23374=CARTESIAN_POINT('Origin',(13.3346225254169,0.,0.));
#23375=CARTESIAN_POINT('Ctrl Pts',(6.11626248314343,2.84862442585767,-1.50713517738359));
#23376=CARTESIAN_POINT('Ctrl Pts',(6.10982035582423,2.79982088127992,-1.59937837576342));
#23377=CARTESIAN_POINT('Ctrl Pts',(6.10337822850504,2.74652053778117,-1.68927261412125));
#23378=CARTESIAN_POINT('Ctrl Pts',(6.09693610118584,2.68897491888786,-1.77638156038956));
#23379=CARTESIAN_POINT('Ctrl Pts',(6.09049542621811,2.63144227342083,-1.86347086829939));
#23380=CARTESIAN_POINT('Ctrl Pts',(6.08405475125038,2.56966646883176,-1.94777581926405));
#23381=CARTESIAN_POINT('Ctrl Pts',(6.07761407628265,2.50394281760817,-2.02888834799959));
#23382=CARTESIAN_POINT('Ctrl Pts',(6.07117396043016,2.43822487185728,-2.10999383535336));
#23383=CARTESIAN_POINT('Ctrl Pts',(6.06473384457767,2.3685600017985,-2.18790715876599));
#23384=CARTESIAN_POINT('Ctrl Pts',(6.05829372872518,2.29528410403912,-2.26225295761666));
#23385=CARTESIAN_POINT('Ctrl Pts',(6.05185327926446,2.22200441047183,-2.33660260769782));
#23386=CARTESIAN_POINT('Ctrl Pts',(6.04541282980374,2.14511358362727,-2.40738409599932));
#23387=CARTESIAN_POINT('Ctrl Pts',(6.03897238034302,2.06498444621732,-2.47425883839596));
#23388=CARTESIAN_POINT('Ctrl Pts',(6.03252855005019,1.9848132460348,-2.54116868583893));
#23389=CARTESIAN_POINT('Ctrl Pts',(6.02608471975735,1.9014006298802,-2.6041674462957));
#23390=CARTESIAN_POINT('Ctrl Pts',(6.01964088946452,1.81515268946992,-2.66295667940921));
#23391=CARTESIAN_POINT('Ctrl Pts',(6.01319552663167,1.72888423666039,-2.72175989440119));
#23392=CARTESIAN_POINT('Ctrl Pts',(6.00675016379883,1.6397794329097,-2.77635137873808));
#23393=CARTESIAN_POINT('Ctrl Pts',(6.00030480096598,1.54827270906505,-2.82647646034146));
#23394=CARTESIAN_POINT('Ctrl Pts',(5.99385464874034,1.45669798879331,-2.87663878867724));
#23395=CARTESIAN_POINT('Ctrl Pts',(5.9874044965147,1.36271811887205,-2.92232790764606));
#23396=CARTESIAN_POINT('Ctrl Pts',(5.98095434428906,1.2667916062669,-2.96333538243509));
#23397=CARTESIAN_POINT('Ctrl Pts',(5.97812664473545,1.22473812483214,-2.98131275941767));
#23398=CARTESIAN_POINT('Ctrl Pts',(5.97529894518185,1.18231078976918,-2.99839099999396));
#23399=CARTESIAN_POINT('Ctrl Pts',(5.97247124562824,1.13954936768589,-3.01455548980388));
#23400=CARTESIAN_POINT('Ctrl Pts',(5.96616787538459,1.04422768643007,-3.05058858389328));
#23401=CARTESIAN_POINT('Ctrl Pts',(5.95986450514094,0.947116827229342,-3.08212614604685));
#23402=CARTESIAN_POINT('Ctrl Pts',(5.95356113489729,0.848668314441946,-3.1089997836221));
#23403=CARTESIAN_POINT('Ctrl Pts',(5.9472619449681,0.750285091448085,-3.1358555989449));
#23404=CARTESIAN_POINT('Ctrl Pts',(5.94096275503892,0.650566373990987,-3.15805353625163));
#23405=CARTESIAN_POINT('Ctrl Pts',(5.93466356510973,0.549979677785018,-3.17547475450892));
#23406=CARTESIAN_POINT('Ctrl Pts',(5.92836715532296,0.449437375436762,-3.1928882839255));
#23407=CARTESIAN_POINT('Ctrl Pts',(5.9220707455362,0.348028259806088,-3.2055292203786));
#23408=CARTESIAN_POINT('Ctrl Pts',(5.91577433574944,0.246230218691873,-3.21332977484462));
#23409=CARTESIAN_POINT('Ctrl Pts',(5.90947930877286,0.144454534344897,-3.22112861616195));
#23410=CARTESIAN_POINT('Ctrl Pts',(5.90318428179628,0.0422905027743748,
-3.22408916141321));
#23411=CARTESIAN_POINT('Ctrl Pts',(5.8968892548197,-0.0597793703575645,
-3.22219552314562));
#23412=CARTESIAN_POINT('Ctrl Pts',(5.89059209293653,-0.161883859646896,
-3.22030124266619));
#23413=CARTESIAN_POINT('Ctrl Pts',(5.88429493105337,-0.263893716779201,
-3.2135494928278));
#23414=CARTESIAN_POINT('Ctrl Pts',(5.8779977691702,-0.365327145324713,-3.20197652074291));
#23415=CARTESIAN_POINT('Ctrl Pts',(5.87169961696178,-0.466776525832027,
-3.19040172863073));
#23416=CARTESIAN_POINT('Ctrl Pts',(5.86540146475336,-0.567648890954547,
-3.17400425846124));
#23417=CARTESIAN_POINT('Ctrl Pts',(5.85910331254494,-0.667469540774835,
-3.15287202002204));
#23418=CARTESIAN_POINT('Ctrl Pts',(5.85279980886301,-0.767375007148562,
-3.13172182574269));
#23419=CARTESIAN_POINT('Ctrl Pts',(5.84649630518108,-0.866226573654231,
-3.10582891961319));
#23420=CARTESIAN_POINT('Ctrl Pts',(5.84019280149915,-0.963561692753684,
-3.07533192139607));
#23421=CARTESIAN_POINT('Ctrl Pts',(5.83635520370379,-1.02281969549554,-3.05676522912006));
#23422=CARTESIAN_POINT('Ctrl Pts',(5.83251760590843,-1.08151592530543,-3.03649304338117));
#23423=CARTESIAN_POINT('Ctrl Pts',(5.82868000811307,-1.13954936768585,-3.01455548980389));
#23424=CARTESIAN_POINT('Ctrl Pts',(5.82223010676624,-1.23708694148339,-2.97768475349715));
#23425=CARTESIAN_POINT('Ctrl Pts',(5.81578020541942,-1.33288511130044,-2.93605663404916));
#23426=CARTESIAN_POINT('Ctrl Pts',(5.8093303040726,-1.42647694442399,-2.88985831651429));
#23427=CARTESIAN_POINT('Ctrl Pts',(5.80288429885277,-1.52001224247094,-2.84368790553208));
#23428=CARTESIAN_POINT('Ctrl Pts',(5.79643829363293,-1.61134351954702,-2.79295296362187));
#23429=CARTESIAN_POINT('Ctrl Pts',(5.78999228841309,-1.70002546687168,-2.73788805002829));
#23430=CARTESIAN_POINT('Ctrl Pts',(5.78354928062754,-1.78866617651503,-2.68284874197707));
#23431=CARTESIAN_POINT('Ctrl Pts',(5.77710627284198,-1.87465968941073,-2.62348367385894));
#23432=CARTESIAN_POINT('Ctrl Pts',(5.77066326505643,-1.95758717987831,-2.56007226376055));
#23433=CARTESIAN_POINT('Ctrl Pts',(5.76422235873842,-2.04048762250796,-2.49668153608646));
#23434=CARTESIAN_POINT('Ctrl Pts',(5.75778145242042,-2.12032373491512,-2.42924732695385));
#23435=CARTESIAN_POINT('Ctrl Pts',(5.75134054610242,-2.19670773918908,-2.35809089542511));
#23436=CARTESIAN_POINT('Ctrl Pts',(5.74489989140302,-2.27308875946739,-2.28693724367316));
#23437=CARTESIAN_POINT('Ctrl Pts',(5.73845923670362,-2.34601765950018,-2.21206191394668));
#23438=CARTESIAN_POINT('Ctrl Pts',(5.73201858200422,-2.41514177295116,-2.13382468329672));
#23439=CARTESIAN_POINT('Ctrl Pts',(5.72557848297815,-2.48425992265654,-2.0555942026348));
#23440=CARTESIAN_POINT('Ctrl Pts',(5.71913838395208,-2.54957369178943,-1.97400268573327));
#23441=CARTESIAN_POINT('Ctrl Pts',(5.712698284926,-2.61076956120682,-1.88944432592653));
#23442=CARTESIAN_POINT('Ctrl Pts',(5.7062564935142,-2.67198151221173,-1.80486374513205));
#23443=CARTESIAN_POINT('Ctrl Pts',(5.6998147021024,-2.72907318027611,-1.7173150718364));
#23444=CARTESIAN_POINT('Ctrl Pts',(5.69337291069059,-2.7817734030335,-1.62722287861111));
#23445=CARTESIAN_POINT('Ctrl Pts',(5.69054486399302,-2.80490962111365,-1.58767100348194));
#23446=CARTESIAN_POINT('Ctrl Pts',(5.68771681729545,-2.82720002732681,-1.54762926569109));
#23447=CARTESIAN_POINT('Ctrl Pts',(5.68488877059788,-2.84862442585766,-1.50713517738361));
#23448=CARTESIAN_POINT('Ctrl Pts',(6.36280938168963,2.84862442585767,-1.50713517738359));
#23449=CARTESIAN_POINT('Ctrl Pts',(6.35636801520394,2.79982664511693,-1.59936748158012));
#23450=CARTESIAN_POINT('Ctrl Pts',(6.34992664871825,2.74653302174499,-1.68925157837877));
#23451=CARTESIAN_POINT('Ctrl Pts',(6.34348528223255,2.68899497203504,-1.77635120482135));
#23452=CARTESIAN_POINT('Ctrl Pts',(6.33704537919698,2.63146999471675,-1.86343104261215));
#23453=CARTESIAN_POINT('Ctrl Pts',(6.3306054761614,2.56970272181874,-1.94772735437613));
#23454=CARTESIAN_POINT('Ctrl Pts',(6.32416557312583,2.50398836217138,-2.02883213810564));
#23455=CARTESIAN_POINT('Ctrl Pts',(6.31772623687936,2.43827978617998,-2.10992978363631));
#23456=CARTESIAN_POINT('Ctrl Pts',(6.3112869006329,2.36862505518029,-2.18783616676831));
#23457=CARTESIAN_POINT('Ctrl Pts',(6.30484756438643,2.2953599652657,-2.26217598615922));
#23458=CARTESIAN_POINT('Ctrl Pts',(6.29840789879005,2.2220911280935,-2.33651960777647));
#23459=CARTESIAN_POINT('Ctrl Pts',(6.29196823319366,2.14521183132221,-2.40729603306182));
#23460=CARTESIAN_POINT('Ctrl Pts',(6.28552856759727,2.06509479949499,-2.47416673480158));
#23461=CARTESIAN_POINT('Ctrl Pts',(6.27908551911379,1.9849356805641,-2.54107256507885));
#23462=CARTESIAN_POINT('Ctrl Pts',(6.2726424706303,1.90153571941476,-2.60406832868935));
#23463=CARTESIAN_POINT('Ctrl Pts',(6.26619942214681,1.81530091132731,-2.66285564081763));
#23464=CARTESIAN_POINT('Ctrl Pts',(6.25975483835675,1.72904555444717,-2.72165696130652));
#23465=CARTESIAN_POINT('Ctrl Pts',(6.25331025456669,1.63995432172068,-2.77624762357214));
#23466=CARTESIAN_POINT('Ctrl Pts',(6.24686567077663,1.54846154749456,-2.82637301119841));
#23467=CARTESIAN_POINT('Ctrl Pts',(6.24041628551254,1.45690060747319,-2.87653574425374));
#23468=CARTESIAN_POINT('Ctrl Pts',(6.23396690024845,1.36293488768221,-2.92222638010325));
#23469=CARTESIAN_POINT('Ctrl Pts',(6.22751751498436,1.26702279812037,-2.96323653992442));
#23470=CARTESIAN_POINT('Ctrl Pts',(6.22468439138106,1.22488997558715,-2.98125172230338));
#23471=CARTESIAN_POINT('Ctrl Pts',(6.22185126777775,1.18238182695123,-2.99836432568748));
#23472=CARTESIAN_POINT('Ctrl Pts',(6.21901814417444,1.13953835446524,-3.01455965295143));
#23473=CARTESIAN_POINT('Ctrl Pts',(6.21271358172062,1.04419858612223,-3.05059918616363));
#23474=CARTESIAN_POINT('Ctrl Pts',(6.2064090192668,0.947069335931392,-3.08214135506957));
#23475=CARTESIAN_POINT('Ctrl Pts',(6.20010445681298,0.84860231617677,-3.10901779851442));
#23476=CARTESIAN_POINT('Ctrl Pts',(6.19380406548531,0.750200442633861,-3.13587646038652));
#23477=CARTESIAN_POINT('Ctrl Pts',(6.18750367415763,0.650462954403152,-3.15807543117493));
#23478=CARTESIAN_POINT('Ctrl Pts',(6.18120328282995,0.549857543880931,-3.17549590519925));
#23479=CARTESIAN_POINT('Ctrl Pts',(6.17490566533694,0.449296426286045,-3.19290870961828));
#23480=CARTESIAN_POINT('Ctrl Pts',(6.16860804784393,0.347868549735401,-3.20554713469663));
#23481=CARTESIAN_POINT('Ctrl Pts',(6.16231043035092,0.246051969765162,-3.21334342868525));
#23482=CARTESIAN_POINT('Ctrl Pts',(6.15601419223677,0.144257690869664,-3.22113801503711));
#23483=CARTESIAN_POINT('Ctrl Pts',(6.14971795412262,0.0420752860446296,
-3.22409255138702));
#23484=CARTESIAN_POINT('Ctrl Pts',(6.14342171600848,-0.0600125776946586,
-3.22219118815418));
#23485=CARTESIAN_POINT('Ctrl Pts',(6.13712334637876,-0.162135002050547,
-3.22028918123772));
#23486=CARTESIAN_POINT('Ctrl Pts',(6.13082497674903,-0.264162411682084,
-3.21352799363139));
#23487=CARTESIAN_POINT('Ctrl Pts',(6.12452660711931,-0.365612853322439,
-3.20194391018728));
#23488=CARTESIAN_POINT('Ctrl Pts',(6.11822724939808,-0.467079210560954,
-3.19035800942613));
#23489=CARTESIAN_POINT('Ctrl Pts',(6.11192789167685,-0.567968013507524,
-3.17394776016987));
#23490=CARTESIAN_POINT('Ctrl Pts',(6.10562853395562,-0.667804406318028,
-3.15280110971216));
#23491=CARTESIAN_POINT('Ctrl Pts',(6.09932383828838,-0.767725398431793,
-3.13163654001835));
#23492=CARTESIAN_POINT('Ctrl Pts',(6.09301914262114,-0.86659179974346,-3.10572764459076));
#23493=CARTESIAN_POINT('Ctrl Pts',(6.08671444695391,-0.963940906770531,
-3.07521308054489));
#23494=CARTESIAN_POINT('Ctrl Pts',(6.08288526685569,-1.02306624491239,-3.05667994785821));
#23495=CARTESIAN_POINT('Ctrl Pts',(6.07905608675748,-1.08163217204868,-3.03644885848091));
#23496=CARTESIAN_POINT('Ctrl Pts',(6.07522690665927,-1.13953835446521,-3.01455965295144));
#23497=CARTESIAN_POINT('Ctrl Pts',(6.06877777336206,-1.23706437297518,-2.97769369193402));
#23498=CARTESIAN_POINT('Ctrl Pts',(6.06232864006486,-1.33285164201609,-2.93607139738089));
#23499=CARTESIAN_POINT('Ctrl Pts',(6.05587950676766,-1.42643331191441,-2.88987985375878));
#23500=CARTESIAN_POINT('Ctrl Pts',(6.04943427814655,-1.5199583220893,-2.84371627715297));
#23501=CARTESIAN_POINT('Ctrl Pts',(6.04298904952543,-1.61128005392832,-2.79298913024698));
#23502=CARTESIAN_POINT('Ctrl Pts',(6.03654382090432,-1.69995327473113,-2.73793287467588));
#23503=CARTESIAN_POINT('Ctrl Pts',(6.03010159483563,-1.78858518652693,-2.68290226742595));
#23504=CARTESIAN_POINT('Ctrl Pts',(6.02365936876695,-1.87457072385523,-2.62354676971529));
#23505=CARTESIAN_POINT('Ctrl Pts',(6.01721714269827,-1.9574911320762,-2.56014570490491));
#23506=CARTESIAN_POINT('Ctrl Pts',(6.01077701979519,-2.04038446963108,-2.49676533836522));
#23507=CARTESIAN_POINT('Ctrl Pts',(6.00433689689211,-2.12021437140274,-2.42934226726545));
#23508=CARTESIAN_POINT('Ctrl Pts',(5.99789677398903,-2.19659312725626,-2.35819765833794));
#23509=CARTESIAN_POINT('Ctrl Pts',(5.99145689714146,-2.27296896493357,-2.28705576760744));
#23510=CARTESIAN_POINT('Ctrl Pts',(5.98501702029389,-2.34589363843928,-2.21219287712536));
#23511=CARTESIAN_POINT('Ctrl Pts',(5.97857714344631,-2.41501454690557,-2.13396867379409));
#23512=CARTESIAN_POINT('Ctrl Pts',(5.97213781730877,-2.48412954445493,-2.0557511598536));
#23513=CARTESIAN_POINT('Ctrl Pts',(5.96569849117122,-2.54944117691125,-1.97417319267129));
#23514=CARTESIAN_POINT('Ctrl Pts',(5.95925916503367,-2.61063599032593,-1.88962887586821));
#23515=CARTESIAN_POINT('Ctrl Pts',(5.9528181318071,-2.67184702671059,-1.80506214605598));
#23516=CARTESIAN_POINT('Ctrl Pts',(5.94637709858052,-2.72893884225502,-1.71752780370473));
#23517=CARTESIAN_POINT('Ctrl Pts',(5.93993606535394,-2.78164033975134,-1.62745033188975));
#23518=CARTESIAN_POINT('Ctrl Pts',(5.93710259995065,-2.80482417759292,-1.58782448444805));
#23519=CARTESIAN_POINT('Ctrl Pts',(5.93426913454737,-2.82715897690467,-1.54770685477331));
#23520=CARTESIAN_POINT('Ctrl Pts',(5.93143566914408,-2.84862442585766,-1.50713517738361));
#23521=CARTESIAN_POINT('Origin',(13.3346225254169,0.,0.));
#23522=CARTESIAN_POINT('Ctrl Pts',(6.98780938168963,-2.84862442585767,1.50713517738359));
#23523=CARTESIAN_POINT('Ctrl Pts',(6.9813684199558,-2.79982971139062,1.59936168604016));
#23524=CARTESIAN_POINT('Ctrl Pts',(6.97492745822197,-2.74653966288739,1.68924038781867));
#23525=CARTESIAN_POINT('Ctrl Pts',(6.96848649648814,-2.68900563955951,1.77633505649051));
#23526=CARTESIAN_POINT('Ctrl Pts',(6.96204700411376,-2.63148474131515,1.86340985648754));
#23527=CARTESIAN_POINT('Ctrl Pts',(6.95560751173937,-2.56972200671623,1.94770157259629));
#23528=CARTESIAN_POINT('Ctrl Pts',(6.94916801936499,-2.50401258941778,2.0288022364285));
#23529=CARTESIAN_POINT('Ctrl Pts',(6.94272909787128,-2.43830899745991,2.1098957104391));
#23530=CARTESIAN_POINT('Ctrl Pts',(6.93629017637757,-2.3686596595625,2.18779840172598));
#23531=CARTESIAN_POINT('Ctrl Pts',(6.92985125488386,-2.29540031832038,2.26213504043298));
#23532=CARTESIAN_POINT('Ctrl Pts',(6.92341200631891,-2.22213725579923,2.33647545514137));
#23533=CARTESIAN_POINT('Ctrl Pts',(6.91697275775396,-2.14526409186646,2.40724918715468));
#23534=CARTESIAN_POINT('Ctrl Pts',(6.91053350918901,-2.06515349881969,2.47411773948064));
#23535=CARTESIAN_POINT('Ctrl Pts',(6.90409087667113,-1.98500080606625,2.54102143255805));
#23536=CARTESIAN_POINT('Ctrl Pts',(6.89764824415326,-1.90160757612952,2.60401560177531));
#23537=CARTESIAN_POINT('Ctrl Pts',(6.89120561163538,-1.81537975297001,2.66280189180618));
#23538=CARTESIAN_POINT('Ctrl Pts',(6.88476144235891,-1.72913136192184,2.72160220410762));
#23539=CARTESIAN_POINT('Ctrl Pts',(6.87831727308244,-1.64004734757743,2.77619242868343));
#23540=CARTESIAN_POINT('Ctrl Pts',(6.87187310380597,-1.54856199293611,2.82631797866655));
#23541=CARTESIAN_POINT('Ctrl Pts',(6.8654241266606,-1.45700838285753,2.87648092634403));
#23542=CARTESIAN_POINT('Ctrl Pts',(6.85897514951523,-1.36305018959993,2.92217236843239));
#23543=CARTESIAN_POINT('Ctrl Pts',(6.85252617236985,-1.2671457715718,2.9631839558299));
#23544=CARTESIAN_POINT('Ctrl Pts',(6.84969016297138,-1.22497073749248,2.98121925734884));
#23545=CARTESIAN_POINT('Ctrl Pts',(6.84685415357291,-1.18241959261408,2.99835014558505));
#23546=CARTESIAN_POINT('Ctrl Pts',(6.84401814417444,-1.13953246495152,3.01456187924904));
#23547=CARTESIAN_POINT('Ctrl Pts',(6.8377129402968,-1.04418296301259,3.05060487897125));
#23548=CARTESIAN_POINT('Ctrl Pts',(6.83140773641917,-0.947043815550281,
3.08214952814751));
#23549=CARTESIAN_POINT('Ctrl Pts',(6.82510253254154,-0.848566836014205,
3.10902748256056));
#23550=CARTESIAN_POINT('Ctrl Pts',(6.81880149482907,-0.750154925168804,
3.13588767735801));
#23551=CARTESIAN_POINT('Ctrl Pts',(6.81250045711659,-0.650407334833339,
3.15808720518624));
#23552=CARTESIAN_POINT('Ctrl Pts',(6.80619941940412,-0.54979185252027,3.1755072793811));
#23553=CARTESIAN_POINT('Ctrl Pts',(6.79990115212197,-0.449220608663864,
3.19291969434519));
#23554=CARTESIAN_POINT('Ctrl Pts',(6.79360288483982,-0.347782635016613,
3.20555676842139));
#23555=CARTESIAN_POINT('Ctrl Pts',(6.78730461755768,-0.245956077419378,
3.21335076990989));
#23556=CARTESIAN_POINT('Ctrl Pts',(6.78100772780445,-0.144151790872555,
3.22114306672915));
#23557=CARTESIAN_POINT('Ctrl Pts',(6.77471083805123,-0.0419594974512284,
3.22409436944162));
#23558=CARTESIAN_POINT('Ctrl Pts',(6.768413948298,0.060138048957664,3.2221888488367));
#23559=CARTESIAN_POINT('Ctrl Pts',(6.76211492886047,0.162270125992154,3.22028268376165));
#23560=CARTESIAN_POINT('Ctrl Pts',(6.75581590942294,0.264306982419248,3.21351641681952));
#23561=CARTESIAN_POINT('Ctrl Pts',(6.74951688998541,0.365766580528667,3.20192635316123));
#23562=CARTESIAN_POINT('Ctrl Pts',(6.74321688366827,0.467242074510221,3.19033447366517));
#23563=CARTESIAN_POINT('Ctrl Pts',(6.73691687735114,0.568139724143099,3.173917346508));
#23564=CARTESIAN_POINT('Ctrl Pts',(6.73061687103401,0.667984589626474,3.15276293915695));
#23565=CARTESIAN_POINT('Ctrl Pts',(6.72431153406959,0.767913937209478,3.13159063235017));
#23566=CARTESIAN_POINT('Ctrl Pts',(6.71800619710517,0.86678832208374,3.10567313109845));
#23567=CARTESIAN_POINT('Ctrl Pts',(6.71170086014075,0.964144956797867,3.07514911260921));
#23568=CARTESIAN_POINT('Ctrl Pts',(6.70787620898025,1.02319892457826,3.05663404776865));
#23569=CARTESIAN_POINT('Ctrl Pts',(6.70405155781976,1.08169475021288,3.03642507406251));
#23570=CARTESIAN_POINT('Ctrl Pts',(6.70022690665927,1.13953246495153,3.01456187924904));
#23571=CARTESIAN_POINT('Ctrl Pts',(6.6937781820509,1.23705233766024,2.9776984591632));
#23572=CARTESIAN_POINT('Ctrl Pts',(6.68732945744253,1.33283380889837,2.93607926380706));
#23573=CARTESIAN_POINT('Ctrl Pts',(6.68088073283417,1.42641007316879,2.88989132419588));
#23574=CARTESIAN_POINT('Ctrl Pts',(6.6744359174242,1.51992961177559,2.84373138358152));
#23575=CARTESIAN_POINT('Ctrl Pts',(6.66799110201424,1.61124626690784,2.79300838362011));
#23576=CARTESIAN_POINT('Ctrl Pts',(6.66154628660428,1.69991484634418,2.73795673407719));
#23577=CARTESIAN_POINT('Ctrl Pts',(6.65510447644813,1.78854207912121,2.68293075542934));
#23578=CARTESIAN_POINT('Ctrl Pts',(6.64866266629199,1.8745233746496,2.62358034887997));
#23579=CARTESIAN_POINT('Ctrl Pts',(6.64222085613585,1.95744001609221,2.56018478745205));
#23580=CARTESIAN_POINT('Ctrl Pts',(6.63578115003153,2.04032957494374,2.49680993255586));
#23581=CARTESIAN_POINT('Ctrl Pts',(6.6293414439272,2.12015617361231,2.42939278637265));
#23582=CARTESIAN_POINT('Ctrl Pts',(6.62290173782288,2.19653213803325,2.35825446656782));
#23583=CARTESIAN_POINT('Ctrl Pts',(6.61646227479629,2.27290521951257,2.28711883200074));
#23584=CARTESIAN_POINT('Ctrl Pts',(6.61002281176971,2.34582764520509,2.21226255849171));
#23585=CARTESIAN_POINT('Ctrl Pts',(6.60358334874312,2.41494684908908,2.13404528503374));
#23586=CARTESIAN_POINT('Ctrl Pts',(6.59714443377973,2.48406017023226,2.05583466865398));
#23587=CARTESIAN_POINT('Ctrl Pts',(6.59070551881635,2.54937066628114,1.9742639092255));
#23588=CARTESIAN_POINT('Ctrl Pts',(6.58426660385296,2.61056491799165,1.88972706268689));
#23589=CARTESIAN_POINT('Ctrl Pts',(6.57782597397146,2.6717754679654,1.80516770089988));
#23590=CARTESIAN_POINT('Ctrl Pts',(6.57138534408995,2.72886736191435,1.71764098199117));
#23591=CARTESIAN_POINT('Ctrl Pts',(6.56494471420844,2.78156953731932,1.6275713414647));
#23592=CARTESIAN_POINT('Ctrl Pts',(6.56210836585366,2.80477871580865,1.58790614078966));
#23593=CARTESIAN_POINT('Ctrl Pts',(6.55927201749887,2.8271371365645,1.54774813502967));
#23594=CARTESIAN_POINT('Ctrl Pts',(6.55643566914408,2.84862442585766,1.50713517738362));
#23595=CARTESIAN_POINT('Ctrl Pts',(6.74126248314343,-2.84862442585767,1.50713517738358));
#23596=CARTESIAN_POINT('Ctrl Pts',(6.7348208129161,-2.79982434406511,1.59937183078017));
#23597=CARTESIAN_POINT('Ctrl Pts',(6.72837914268876,-2.74652803790824,1.68925997627709));
#23598=CARTESIAN_POINT('Ctrl Pts',(6.72193747246143,-2.68898696649982,1.77636332333621));
#23599=CARTESIAN_POINT('Ctrl Pts',(6.71549726125213,-2.63145892796298,1.86344694176137));
#23600=CARTESIAN_POINT('Ctrl Pts',(6.70905705004283,-2.56968824914852,1.94774670241053));
#23601=CARTESIAN_POINT('Ctrl Pts',(6.70261683883353,-2.50397018027766,2.02885457802679));
#23602=CARTESIAN_POINT('Ctrl Pts',(6.69617719134728,-2.43825786382539,2.1099553541275));
#23603=CARTESIAN_POINT('Ctrl Pts',(6.68973754386104,-2.36859908529649,2.18786450789556));
#23604=CARTESIAN_POINT('Ctrl Pts',(6.68329789637479,-2.29532968091904,2.26220671433716));
#23605=CARTESIAN_POINT('Ctrl Pts',(6.6768579178349,-2.22205650985969,2.33655274261197));
#23606=CARTESIAN_POINT('Ctrl Pts',(6.67041793929501,-2.14517261031037,2.40733118911841));
#23607=CARTESIAN_POINT('Ctrl Pts',(6.66397796075512,-2.06505074601119,2.47420350393791));
#23608=CARTESIAN_POINT('Ctrl Pts',(6.6575346001408,-1.98488680422579,2.54111093799645));
#23609=CARTESIAN_POINT('Ctrl Pts',(6.65109123952648,-1.90148179122128,2.60410789805176));
#23610=CARTESIAN_POINT('Ctrl Pts',(6.64464787891216,-1.81524174078208,2.66289597713137));
#23611=CARTESIAN_POINT('Ctrl Pts',(6.63820298409013,-1.72898115600406,2.72169805404991));
#23612=CARTESIAN_POINT('Ctrl Pts',(6.63175808926811,-1.63988450576559,2.7762890446133));
#23613=CARTESIAN_POINT('Ctrl Pts',(6.62531319444608,-1.54838616294132,2.8264143102015));
#23614=CARTESIAN_POINT('Ctrl Pts',(6.61886350296394,-1.45681972180614,2.87657688188527));
#23615=CARTESIAN_POINT('Ctrl Pts',(6.61241381148181,-1.36284835328739,2.92226691237498));
#23616=CARTESIAN_POINT('Ctrl Pts',(6.60596411999967,-1.26693050609646,2.96327600051399));
#23617=CARTESIAN_POINT('Ctrl Pts',(6.60313316187586,-1.22482935916943,2.98127608804355));
#23618=CARTESIAN_POINT('Ctrl Pts',(6.60030220375205,-1.18235347438299,2.9983749717808));
#23619=CARTESIAN_POINT('Ctrl Pts',(6.59747124562824,-1.1395427597969,3.01455798768152));
#23620=CARTESIAN_POINT('Ctrl Pts',(6.59116716115003,-1.04421024355315,3.05059493873793));
#23621=CARTESIAN_POINT('Ctrl Pts',(6.58486307667181,-0.947088367349843,
3.08213526022758));
#23622=CARTESIAN_POINT('Ctrl Pts',(6.5785589921936,-0.848628768111771,3.10901057837266));
#23623=CARTESIAN_POINT('Ctrl Pts',(6.57225908253034,-0.750234372728276,
3.13586809861535));
#23624=CARTESIAN_POINT('Ctrl Pts',(6.56595917286709,-0.650504410890921,
3.15806665478402));
#23625=CARTESIAN_POINT('Ctrl Pts',(6.55965926320383,-0.549906504144592,
3.17548742702589));
#23626=CARTESIAN_POINT('Ctrl Pts',(6.55336212990721,-0.44935293083903,3.19290052194325));
#23627=CARTESIAN_POINT('Ctrl Pts',(6.54706499661059,-0.347932576815247,
3.20553995383521));
#23628=CARTESIAN_POINT('Ctrl Pts',(6.54076786331396,-0.246123430343797,
3.2133379560102));
#23629=CARTESIAN_POINT('Ctrl Pts',(6.53447211077298,-0.144336607292632,
3.22113424833802));
#23630=CARTESIAN_POINT('Ctrl Pts',(6.528176358232,-0.0421615695926382,3.22409119397625));
#23631=CARTESIAN_POINT('Ctrl Pts',(6.52188060569102,0.0599190804475121,
3.22219292816217));
#23632=CARTESIAN_POINT('Ctrl Pts',(6.51558272027298,0.162034313402983,3.220294019253));
#23633=CARTESIAN_POINT('Ctrl Pts',(6.50928483485493,0.264054685027798,3.21353661588369));
#23634=CARTESIAN_POINT('Ctrl Pts',(6.50298694943689,0.365498304951598,3.20195698777755));
#23635=CARTESIAN_POINT('Ctrl Pts',(6.49668807502886,0.466957855099198,3.19037554126167));
#23636=CARTESIAN_POINT('Ctrl Pts',(6.49038920062083,0.567840067045023,3.17397041608279));
#23637=CARTESIAN_POINT('Ctrl Pts',(6.4840903262128,0.667670147477321,3.15282954449929));
#23638=CARTESIAN_POINT('Ctrl Pts',(6.47778610842939,0.767584914404384,3.13167073897942));
#23639=CARTESIAN_POINT('Ctrl Pts',(6.47148189064597,0.866445367585899,3.10576825487636));
#23640=CARTESIAN_POINT('Ctrl Pts',(6.46517767286255,0.963788866079588,3.07526073433149));
#23641=CARTESIAN_POINT('Ctrl Pts',(6.46134511794606,1.02296739013412,3.05671414348212));
#23642=CARTESIAN_POINT('Ctrl Pts',(6.45751256302956,1.08158555679706,3.03646657637891));
#23643=CARTESIAN_POINT('Ctrl Pts',(6.45368000811307,1.13954275979688,3.01455798768153));
#23644=CARTESIAN_POINT('Ctrl Pts',(6.44723056816595,1.23707339103231,2.97769012010794));
#23645=CARTESIAN_POINT('Ctrl Pts',(6.44078112821883,1.33286501155701,2.93606550000405));
#23646=CARTESIAN_POINT('Ctrl Pts',(6.43433168827171,1.4264507385462,2.88987125197663));
#23647=CARTESIAN_POINT('Ctrl Pts',(6.42788614959502,1.5199798554682,2.84370494687992));
#23648=CARTESIAN_POINT('Ctrl Pts',(6.42144061091833,1.61130539763696,2.79297468800413));
#23649=CARTESIAN_POINT('Ctrl Pts',(6.41499507224163,1.69998210197784,2.73791497593607));
#23650=CARTESIAN_POINT('Ctrl Pts',(6.40855253408015,1.78861752570373,2.68288089516308));
#23651=CARTESIAN_POINT('Ctrl Pts',(6.40210999591867,1.87460624675235,2.62352157678041));
#23652=CARTESIAN_POINT('Ctrl Pts',(6.39566745775719,1.95752948212021,2.56011638195028));
#23653=CARTESIAN_POINT('Ctrl Pts',(6.38922702208823,2.04042565587394,2.49673187911206));
#23654=CARTESIAN_POINT('Ctrl Pts',(6.38278658641927,2.12025803682909,2.42930436156649));
#23655=CARTESIAN_POINT('Ctrl Pts',(6.3763461507503,2.19663888778923,2.35815503289163));
#23656=CARTESIAN_POINT('Ctrl Pts',(6.36990596336282,2.27301679423575,2.28700844705302));
#23657=CARTESIAN_POINT('Ctrl Pts',(6.36346577597533,2.34594315489066,2.2121405907003));
#23658=CARTESIAN_POINT('Ctrl Pts',(6.35702558858784,2.41506534274487,2.13391118671153));
#23659=CARTESIAN_POINT('Ctrl Pts',(6.35058595389354,2.48418159857257,2.05568849632534));
#23660=CARTESIAN_POINT('Ctrl Pts',(6.34414631919925,2.54949408396817,1.97410511993885));
#23661=CARTESIAN_POINT('Ctrl Pts',(6.33770668450495,2.61068931895004,1.88955519697631));
#23662=CARTESIAN_POINT('Ctrl Pts',(6.33126534859332,2.6719007204381,1.80498293768557));
#23663=CARTESIAN_POINT('Ctrl Pts',(6.3248240126817,2.72899247713051,1.71744287422061));
#23664=CARTESIAN_POINT('Ctrl Pts',(6.31838267677007,2.78169346579974,1.62735952537448));
#23665=CARTESIAN_POINT('Ctrl Pts',(6.31555137471267,2.80485829056485,1.58776320957532));
#23666=CARTESIAN_POINT('Ctrl Pts',(6.31272007265528,2.82717536573749,1.54767587836842));
#23667=CARTESIAN_POINT('Ctrl Pts',(6.30988877059788,2.84862442585767,1.5071351773836));
#23668=CARTESIAN_POINT('Origin',(13.3346225254169,0.,0.));
#23669=CARTESIAN_POINT('Ctrl Pts',(7.36626248314343,2.84862442585767,-1.50713517738359));
#23670=CARTESIAN_POINT('Ctrl Pts',(7.3598212383318,2.7998275668816,-1.59936573935991));
#23671=CARTESIAN_POINT('Ctrl Pts',(7.35337999352017,2.74653501817546,-1.6892482143296));
#23672=CARTESIAN_POINT('Ctrl Pts',(7.34693874870854,2.68899817887566,-1.77634635037861));
#23673=CARTESIAN_POINT('Ctrl Pts',(7.34049896912302,2.63147442780365,-1.86342467372571));
#23674=CARTESIAN_POINT('Ctrl Pts',(7.3340591895375,2.56970851921407,-1.94771960395087));
#23675=CARTESIAN_POINT('Ctrl Pts',(7.32761940995198,2.50399564535328,-2.02882314915614));
#23676=CARTESIAN_POINT('Ctrl Pts',(7.32118019838482,2.438288567672,-2.10991954065347));
#23677=CARTESIAN_POINT('Ctrl Pts',(7.31474098681766,2.36863545796846,-2.18782481394358));
#23678=CARTESIAN_POINT('Ctrl Pts',(7.30830177525049,2.29537209625576,-2.26216367715301));
#23679=CARTESIAN_POINT('Ctrl Pts',(7.30186223501736,2.22210499508307,-2.33650633471747));
#23680=CARTESIAN_POINT('Ctrl Pts',(7.29542269478422,2.14522754200268,-2.40728195035351));
#23681=CARTESIAN_POINT('Ctrl Pts',(7.28898315455109,2.0651124458537,-2.47415200593661));
#23682=CARTESIAN_POINT('Ctrl Pts',(7.28254023110834,1.9849552587862,-2.54105719375067));
#23683=CARTESIAN_POINT('Ctrl Pts',(7.2760973076656,1.90155732121291,-2.6040524780719));
#23684=CARTESIAN_POINT('Ctrl Pts',(7.26965438422285,1.81532461298809,-2.66283948295417));
#23685=CARTESIAN_POINT('Ctrl Pts',(7.26320992503554,1.72907135020997,-2.72164050039212));
#23686=CARTESIAN_POINT('Ctrl Pts',(7.25676546584822,1.63998228752049,-2.77623103110752));
#23687=CARTESIAN_POINT('Ctrl Pts',(7.2503210066609,1.54849174383152,-2.82635646757192));
#23688=CARTESIAN_POINT('Ctrl Pts',(7.24387174407473,1.45693300736477,-2.87651926519532));
#23689=CARTESIAN_POINT('Ctrl Pts',(7.23742248148855,1.36296955024028,-2.92221014346359));
#23690=CARTESIAN_POINT('Ctrl Pts',(7.23097321890238,1.26705976694849,-2.96322073249369));
#23691=CARTESIAN_POINT('Ctrl Pts',(7.228139227811,1.22491425530386,-2.98124196242664));
#23692=CARTESIAN_POINT('Ctrl Pts',(7.22530523671962,1.18239318176599,-2.99836006216386));
#23693=CARTESIAN_POINT('Ctrl Pts',(7.22247124562824,1.1395365863639,-3.01456032131356));
#23694=CARTESIAN_POINT('Ctrl Pts',(7.21616649090883,1.04419390058717,-3.05060089343833));
#23695=CARTESIAN_POINT('Ctrl Pts',(7.20986173618941,0.947061683914143,-3.08214380566377));
#23696=CARTESIAN_POINT('Ctrl Pts',(7.20355698147,0.848591678948619,-3.10902070191229));
#23697=CARTESIAN_POINT('Ctrl Pts',(7.19725639639098,0.75018679697814,-3.13587982316442));
#23698=CARTESIAN_POINT('Ctrl Pts',(7.19095581131196,0.650446280904561,-3.15807896084573));
#23699=CARTESIAN_POINT('Ctrl Pts',(7.18465522623294,0.549837851630633,-3.17549931497618));
#23700=CARTESIAN_POINT('Ctrl Pts',(7.17835741396893,0.449273698969032,-3.19291200260919));
#23701=CARTESIAN_POINT('Ctrl Pts',(7.17205960170492,0.347842796098622,-3.20555002271385));
#23702=CARTESIAN_POINT('Ctrl Pts',(7.16576178944092,0.246023225619735,-3.21334562955118));
#23703=CARTESIAN_POINT('Ctrl Pts',(7.15946535600154,0.144225947220338,-3.22113952964111));
#23704=CARTESIAN_POINT('Ctrl Pts',(7.15316892256216,0.0420405785782795,
-3.22409309677057));
#23705=CARTESIAN_POINT('Ctrl Pts',(7.14687248912278,-0.0600501872561559,
-3.22219048746509));
#23706=CARTESIAN_POINT('Ctrl Pts',(7.14057392471624,-0.162175504725535,
-3.22028723423984));
#23707=CARTESIAN_POINT('Ctrl Pts',(7.1342753603097,-0.264205745761719,-3.21352452423829));
#23708=CARTESIAN_POINT('Ctrl Pts',(7.12797679590316,-0.365658931790838,
-3.2019386483975));
#23709=CARTESIAN_POINT('Ctrl Pts',(7.12167724376763,-0.467128027517231,
-3.1903509556815));
#23710=CARTESIAN_POINT('Ctrl Pts',(7.1153776916321,-0.568019482016492,-3.17393864498104));
#23711=CARTESIAN_POINT('Ctrl Pts',(7.10907813949657,-0.667858414283587,
-3.15278966963713));
#23712=CARTESIAN_POINT('Ctrl Pts',(7.10277325160128,-0.767781910746003,
-3.13162278097984));
#23713=CARTESIAN_POINT('Ctrl Pts',(7.09646836370599,-0.866650704941091,
-3.10571130622614));
#23714=CARTESIAN_POINT('Ctrl Pts',(7.09016347581069,-0.964002068221984,
-3.07519390851435));
#23715=CARTESIAN_POINT('Ctrl Pts',(7.08633565324482,-1.02310601287161,-3.0566661907257));
#23716=CARTESIAN_POINT('Ctrl Pts',(7.08250783067894,-1.08165092699262,-3.03644173009248));
#23717=CARTESIAN_POINT('Ctrl Pts',(7.07868000811307,-1.13953658636387,-3.01456032131357));
#23718=CARTESIAN_POINT('Ctrl Pts',(7.07223099766582,-1.2370607572487,-2.97769512409316));
#23719=CARTESIAN_POINT('Ctrl Pts',(7.06578198721857,-1.33284628329249,-2.93607376116759));
#23720=CARTESIAN_POINT('Ctrl Pts',(7.05933297677132,-1.42642632810164,-2.88988330093076));
#23721=CARTESIAN_POINT('Ctrl Pts',(7.05288787236158,-1.51994969333675,-2.84372081733806));
#23722=CARTESIAN_POINT('Ctrl Pts',(7.04644276795183,-1.61126989895293,-2.79299491705124));
#23723=CARTESIAN_POINT('Ctrl Pts',(7.03999766354209,-1.69994172441788,-2.73794004610824));
#23724=CARTESIAN_POINT('Ctrl Pts',(7.03355556249848,-1.78857222953475,-2.68291083028645));
#23725=CARTESIAN_POINT('Ctrl Pts',(7.02711346145488,-1.87455649163518,-2.62355686305991));
#23726=CARTESIAN_POINT('Ctrl Pts',(7.02067136041127,-1.95747576744255,-2.5601574526531));
#23727=CARTESIAN_POINT('Ctrl Pts',(7.01423136280101,-2.04036796898196,-2.4967787430135));
#23728=CARTESIAN_POINT('Ctrl Pts',(7.00779136519075,-2.12019687772764,-2.42935745305116));
#23729=CARTESIAN_POINT('Ctrl Pts',(7.00135136758049,-2.19657479438669,-2.35821473474428));
#23730=CARTESIAN_POINT('Ctrl Pts',(6.99491161513201,-2.27294980344431,-2.28707472474209));
#23731=CARTESIAN_POINT('Ctrl Pts',(6.98847186268353,-2.34587380117559,-2.21221382345213));
#23732=CARTESIAN_POINT('Ctrl Pts',(6.98203211023506,-2.41499419718648,-2.13399170337085));
#23733=CARTESIAN_POINT('Ctrl Pts',(6.97559290770146,-2.48410869074474,-2.05577626297292));
#23734=CARTESIAN_POINT('Ctrl Pts',(6.96915370516785,-2.54941998155791,-1.97420046257777));
#23735=CARTESIAN_POINT('Ctrl Pts',(6.96271450263425,-2.61061462610829,-1.88965839146908));
#23736=CARTESIAN_POINT('Ctrl Pts',(6.9562735906587,-2.67182551625611,-1.80509387662426));
#23737=CARTESIAN_POINT('Ctrl Pts',(6.94983267868315,-2.72891735537074,-1.71756182601585));
#23738=CARTESIAN_POINT('Ctrl Pts',(6.9433917667076,-2.78161905667021,-1.62748670841551));
#23739=CARTESIAN_POINT('Ctrl Pts',(6.94055743467103,-2.80481051169119,-1.58784903094343));
#23740=CARTESIAN_POINT('Ctrl Pts',(6.93772310263445,-2.82715241156155,-1.54771926387705));
#23741=CARTESIAN_POINT('Ctrl Pts',(6.93488877059788,-2.84862442585766,-1.50713517738361));
#23742=CARTESIAN_POINT('Ctrl Pts',(7.61280938168963,2.84862442585768,-1.50713517738358));
#23743=CARTESIAN_POINT('Ctrl Pts',(7.60636879765673,2.79983257273495,-1.5993562778356));
#23744=CARTESIAN_POINT('Ctrl Pts',(7.59992821362384,2.74654586008821,-1.68922994525756));
#23745=CARTESIAN_POINT('Ctrl Pts',(7.59348762959095,2.68901559383708,-1.77631998767143));
#23746=CARTESIAN_POINT('Ctrl Pts',(7.58704852043615,2.63149850187716,-1.86339008667715));
#23747=CARTESIAN_POINT('Ctrl Pts',(7.58060941128135,2.56974000198426,-1.9476775144583));
#23748=CARTESIAN_POINT('Ctrl Pts',(7.57417030212655,2.504035196303,-2.0287743339701));
#23749=CARTESIAN_POINT('Ctrl Pts',(7.5677317676774,2.43833625493031,-2.10986391539985));
#23750=CARTESIAN_POINT('Ctrl Pts',(7.56129323322826,2.36869194922073,-2.18776316177445));
#23751=CARTESIAN_POINT('Ctrl Pts',(7.55485469877911,2.29543797182663,-2.26209683258618));
#23752=CARTESIAN_POINT('Ctrl Pts',(7.54841583939461,2.22218029750323,-2.33643425481643));
#23753=CARTESIAN_POINT('Ctrl Pts',(7.54197698001011,2.14531285588115,-2.40720547368891));
#23754=CARTESIAN_POINT('Ctrl Pts',(7.53553812062562,2.06520827048847,-2.47407202037573));
#23755=CARTESIAN_POINT('Ctrl Pts',(7.52909587631248,1.98506157386324,-2.54097371901651));
#23756=CARTESIAN_POINT('Ctrl Pts',(7.52265363199935,1.90167462457078,-2.60396640034054));
#23757=CARTESIAN_POINT('Ctrl Pts',(7.51621138768622,1.81545331866872,-2.66275173650018));
#23758=CARTESIAN_POINT('Ctrl Pts',(7.50976760527285,1.72921142723714,-2.72155110779024));
#23759=CARTESIAN_POINT('Ctrl Pts',(7.50332382285949,1.6401341480468,-2.77614092371629));
#23760=CARTESIAN_POINT('Ctrl Pts',(7.49688004044613,1.54865571617306,-2.82626662494261));
#23761=CARTESIAN_POINT('Ctrl Pts',(7.490431444218,1.45710894551977,-2.87642977247378));
#23762=CARTESIAN_POINT('Ctrl Pts',(7.48398284798987,1.36315777501308,-2.92212196647321));
#23763=CARTESIAN_POINT('Ctrl Pts',(7.47753425176174,1.26726051491456,-2.96313488552892));
#23764=CARTESIAN_POINT('Ctrl Pts',(7.47469554923264,1.22504608790665,-2.98118896628243));
#23765=CARTESIAN_POINT('Ctrl Pts',(7.47185684670354,1.18245481698266,-2.99833692023175));
#23766=CARTESIAN_POINT('Ctrl Pts',(7.46901814417444,1.1395269477687,-3.01456396478976));
#23767=CARTESIAN_POINT('Ctrl Pts',(7.46271233675157,1.04416828529453,-3.05061022781874));
#23768=CARTESIAN_POINT('Ctrl Pts',(7.4564065293287,0.94701982317167,-3.08215721203173));
#23769=CARTESIAN_POINT('Ctrl Pts',(7.45010072190583,0.848533470080481,-3.10903658914674));
#23770=CARTESIAN_POINT('Ctrl Pts',(7.44379907596876,0.750112112561231,-3.1358982273524));
#23771=CARTESIAN_POINT('Ctrl Pts',(7.43749743003169,0.650355014495849,-3.15809828004157));
#23772=CARTESIAN_POINT('Ctrl Pts',(7.43119578409462,0.549730052935245,-3.17551797844065));
#23773=CARTESIAN_POINT('Ctrl Pts',(7.42489690537768,0.449149278468226,-3.19293002738744));
#23774=CARTESIAN_POINT('Ctrl Pts',(7.41859802666074,0.347701801609882,-3.20556583037678));
#23775=CARTESIAN_POINT('Ctrl Pts',(7.4122991479438,0.245865853212699,-3.21335767457095));
#23776=CARTESIAN_POINT('Ctrl Pts',(7.4060016450126,0.144052147575286,-3.22114781688949));
#23777=CARTESIAN_POINT('Ctrl Pts',(7.3997041420814,0.0418505470841928,-3.22409607643666));
#23778=CARTESIAN_POINT('Ctrl Pts',(7.3934066391502,-0.0602561125912675,
-3.22218664316569));
#23779=CARTESIAN_POINT('Ctrl Pts',(7.38710700826225,-0.162397274601838,
-3.22027656468797));
#23780=CARTESIAN_POINT('Ctrl Pts',(7.38080737737429,-0.264443022243322,
-3.2135055172559));
#23781=CARTESIAN_POINT('Ctrl Pts',(7.37450774648634,-0.365911238306918,
-3.20190982511699));
#23782=CARTESIAN_POINT('Ctrl Pts',(7.36820712986566,-0.467395331577122,
-3.19031231854586));
#23783=CARTESIAN_POINT('Ctrl Pts',(7.36190651324498,-0.568301307493712,
-3.17388871794434));
#23784=CARTESIAN_POINT('Ctrl Pts',(7.3556058966243,-0.668154147213363,-3.15272700975863));
#23785=CARTESIAN_POINT('Ctrl Pts',(7.34929995623743,-0.768091358543565,
-3.13154742078549));
#23786=CARTESIAN_POINT('Ctrl Pts',(7.34299401585056,-0.866973257105538,
-3.10562181967257));
#23787=CARTESIAN_POINT('Ctrl Pts',(7.33668807546369,-0.964336976392172,
-3.07508890252994));
#23788=CARTESIAN_POINT('Ctrl Pts',(7.33286768586222,-1.02332379166532,-3.05659084641172));
#23789=CARTESIAN_POINT('Ctrl Pts',(7.32904729626074,-1.08175365751474,-3.03640268570416));
#23790=CARTESIAN_POINT('Ctrl Pts',(7.32522690665927,-1.13952694776869,-3.01456396478976));
#23791=CARTESIAN_POINT('Ctrl Pts',(7.31877856349444,-1.23704108642474,-2.97770291619869));
#23792=CARTESIAN_POINT('Ctrl Pts',(7.31233022032962,-1.33281714821767,-2.93608661322007));
#23793=CARTESIAN_POINT('Ctrl Pts',(7.3058818771648,-1.42638836887556,-2.88990203703111));
#23794=CARTESIAN_POINT('Ctrl Pts',(7.2994374474012,-1.51990280258513,-2.84374548955784));
#23795=CARTESIAN_POINT('Ctrl Pts',(7.29299301763761,-1.61121472114748,-2.79302635948626));
#23796=CARTESIAN_POINT('Ctrl Pts',(7.28654858787402,-1.69987897011956,-2.73797900821852));
#23797=CARTESIAN_POINT('Ctrl Pts',(7.28010716587054,-1.78850183749525,-2.68295734878599));
#23798=CARTESIAN_POINT('Ctrl Pts',(7.27366574386706,-1.87447917546878,-2.62361169306084));
#23799=CARTESIAN_POINT('Ctrl Pts',(7.26722432186358,-1.95739230248724,-2.56022126712979));
#23800=CARTESIAN_POINT('Ctrl Pts',(7.26078500472703,-2.04027833593858,-2.49685155532233));
#23801=CARTESIAN_POINT('Ctrl Pts',(7.25434568759048,-2.12010185286642,-2.42943993786715));
#23802=CARTESIAN_POINT('Ctrl Pts',(7.24790637045393,-2.19647521287681,-2.35830748667721));
#23803=CARTESIAN_POINT('Ctrl Pts',(7.24146729360321,-2.27284572298322,-2.28717768982453));
#23804=CARTESIAN_POINT('Ctrl Pts',(7.23502821675248,-2.34576605155333,-2.2123275907323));
#23805=CARTESIAN_POINT('Ctrl Pts',(7.22858913990176,-2.41488366509613,-2.13411678371917));
#23806=CARTESIAN_POINT('Ctrl Pts',(7.22215060863931,-2.4839954222467,-2.05591260357204));
#23807=CARTESIAN_POINT('Ctrl Pts',(7.21571207737686,-2.54930485806267,-1.97434856987299));
#23808=CARTESIAN_POINT('Ctrl Pts',(7.20927354611441,-2.6104985857016,-1.88981869409475));
#23809=CARTESIAN_POINT('Ctrl Pts',(7.20283329262207,-2.67170868192873,-1.80526620758855));
#23810=CARTESIAN_POINT('Ctrl Pts',(7.19639303912973,-2.72880064905917,-1.71774660236723));
#23811=CARTESIAN_POINT('Ctrl Pts',(7.1899527856374,-2.78150345696278,-1.62768426956953));
#23812=CARTESIAN_POINT('Ctrl Pts',(7.18711374680629,-2.80473628752211,-1.58798234474052));
#23813=CARTESIAN_POINT('Ctrl Pts',(7.18427470797519,-2.82711675435621,-1.54778665928234));
#23814=CARTESIAN_POINT('Ctrl Pts',(7.18143566914408,-2.84862442585767,-1.50713517738359));
#23815=CARTESIAN_POINT('Origin',(13.3346225254169,0.,0.));
#23816=CARTESIAN_POINT('Ctrl Pts',(8.23780938168963,-2.84862442585767,1.50713517738358));
#23817=CARTESIAN_POINT('Ctrl Pts',(8.23136915062113,-2.79983524668294,1.59935122382739));
#23818=CARTESIAN_POINT('Ctrl Pts',(8.22492891955262,-2.74655165133479,1.68922018669765));
#23819=CARTESIAN_POINT('Ctrl Pts',(8.21848868848412,-2.6890248959066,1.77630590600113));
#23820=CARTESIAN_POINT('Ctrl Pts',(8.21204993745551,-2.63151136079486,1.86337161199501));
#23821=CARTESIAN_POINT('Ctrl Pts',(8.20561118642689,-2.56975681800966,1.94765503247493));
#23822=CARTESIAN_POINT('Ctrl Pts',(8.19917243539828,-2.50405632153669,2.02874825965967));
#23823=CARTESIAN_POINT('Ctrl Pts',(8.19273426265664,-2.43836172585738,2.10983420357524));
#23824=CARTESIAN_POINT('Ctrl Pts',(8.18629608991499,-2.36872212233407,2.18773023083762));
#23825=CARTESIAN_POINT('Ctrl Pts',(8.17985791717335,-2.29547315692851,2.26206112833421));
#23826=CARTESIAN_POINT('Ctrl Pts',(8.17341942150152,-2.22222051745221,2.33639575416982));
#23827=CARTESIAN_POINT('Ctrl Pts',(8.16698092582969,-2.14535842278167,2.40716462462289));
#23828=CARTESIAN_POINT('Ctrl Pts',(8.16054243015786,-2.06525945085394,2.4740292971504));
#23829=CARTESIAN_POINT('Ctrl Pts',(8.15410054866333,-1.98511835714327,2.54092913191725));
#23830=CARTESIAN_POINT('Ctrl Pts',(8.14765866716881,-1.90173727652333,2.60392042275362));
#23831=CARTESIAN_POINT('Ctrl Pts',(8.14121678567428,-1.81552206027324,2.66270486745362));
#23832=CARTESIAN_POINT('Ctrl Pts',(8.13477336483815,-1.72928624217425,2.72150335918964));
#23833=CARTESIAN_POINT('Ctrl Pts',(8.12832994400202,-1.64021525630153,2.77609279305437));
#23834=CARTESIAN_POINT('Ctrl Pts',(8.12188652316589,-1.54874329293665,2.82621863540026));
#23835=CARTESIAN_POINT('Ctrl Pts',(8.11543828297856,-1.45720291319351,2.87638196932789));
#23836=CARTESIAN_POINT('Ctrl Pts',(8.10899004279122,-1.36325830479589,2.92207486561085));
#23837=CARTESIAN_POINT('Ctrl Pts',(8.10254180260388,-1.26736773300675,2.96308902867149));
#23838=CARTESIAN_POINT('Ctrl Pts',(8.0997005831274,-1.22511649045642,2.98116066302658));
#23839=CARTESIAN_POINT('Ctrl Pts',(8.09685936365092,-1.18248771812384,2.99832456767142));
#23840=CARTESIAN_POINT('Ctrl Pts',(8.09401814417444,-1.13952177176646,3.01456592135091));
#23841=CARTESIAN_POINT('Ctrl Pts',(8.08771176801016,-1.04415447535482,3.05061526092775));
#23842=CARTESIAN_POINT('Ctrl Pts',(8.08140539184588,-0.946997233950487,
3.08216444669572));
#23843=CARTESIAN_POINT('Ctrl Pts',(8.0750990156816,-0.848502046009037,3.10904516538735));
#23844=CARTESIAN_POINT('Ctrl Pts',(8.06879679658347,-0.750071784580219,
3.13590816472276));
#23845=CARTESIAN_POINT('Ctrl Pts',(8.06249457748534,-0.650305724995536,
3.15810871269302));
#23846=CARTESIAN_POINT('Ctrl Pts',(8.05619235838721,-0.549671828716999,
3.17552805738115));
#23847=CARTESIAN_POINT('Ctrl Pts',(8.04989290347794,-0.449082071033278,
3.1929397618464));
#23848=CARTESIAN_POINT('Ctrl Pts',(8.04359344856868,-0.347625636737641,
3.2055743671937));
#23849=CARTESIAN_POINT('Ctrl Pts',(8.03729399365941,-0.245780836828313,
3.213364178357));
#23850=CARTESIAN_POINT('Ctrl Pts',(8.03099591289099,-0.143958252984028,
3.22115229027841));
#23851=CARTESIAN_POINT('Ctrl Pts',(8.02469783212257,-0.0417478798431903,
3.22409768172038));
#23852=CARTESIAN_POINT('Ctrl Pts',(8.01839975135415,0.0603673698212518,
3.22218456069184));
#23853=CARTESIAN_POINT('Ctrl Pts',(8.01209954426089,0.16251709509833,3.22027079376546));
#23854=CARTESIAN_POINT('Ctrl Pts',(8.00579933716762,0.264571223385071,3.21349524051306));
#23855=CARTESIAN_POINT('Ctrl Pts',(7.99949913007435,0.366047562520342,3.20189424317433));
#23856=CARTESIAN_POINT('Ctrl Pts',(7.99319793833492,0.467539761179954,3.19029143274005));
#23857=CARTESIAN_POINT('Ctrl Pts',(7.9868967465955,0.568453585154214,3.17386173043288));
#23858=CARTESIAN_POINT('Ctrl Pts',(7.98059555485607,0.668313941075423,3.15269314058064));
#23859=CARTESIAN_POINT('Ctrl Pts',(7.97428904584675,0.768258564304382,3.13150668758283));
#23860=CARTESIAN_POINT('Ctrl Pts',(7.96798253683744,0.867147544787304,3.10557345163986));
#23861=CARTESIAN_POINT('Ctrl Pts',(7.96167602782812,0.964517941478652,3.07503214667193));
#23862=CARTESIAN_POINT('Ctrl Pts',(7.95785965410517,1.02344147948959,3.0565501253869));
#23863=CARTESIAN_POINT('Ctrl Pts',(7.95404328038221,1.08180919094779,3.03638158040879));
#23864=CARTESIAN_POINT('Ctrl Pts',(7.95022690665925,1.13952177176659,3.01456592135085));
#23865=CARTESIAN_POINT('Ctrl Pts',(7.94377892002184,1.23703055286201,2.97770708930154));
#23866=CARTESIAN_POINT('Ctrl Pts',(7.93733093338443,1.33280156031643,2.93609348956797));
#23867=CARTESIAN_POINT('Ctrl Pts',(7.93088294674702,1.42636806838486,2.88991205679205));
#23868=CARTESIAN_POINT('Ctrl Pts',(7.92443887742247,1.51987773246369,2.84375868038948));
#23869=CARTESIAN_POINT('Ctrl Pts',(7.91799480809792,1.61118522546438,2.7930431668641));
#23870=CARTESIAN_POINT('Ctrl Pts',(7.91155073877338,1.69984542825306,2.73799983245931));
#23871=CARTESIAN_POINT('Ctrl Pts',(7.90510967953751,1.78846421698174,2.6829822093419));
#23872=CARTESIAN_POINT('Ctrl Pts',(7.89866862030166,1.87443785730202,2.62364099324265));
#23873=CARTESIAN_POINT('Ctrl Pts',(7.89222756106579,1.95734770064261,2.5602553664213));
#23874=CARTESIAN_POINT('Ctrl Pts',(7.88578860744736,2.04023044030286,2.49689046070734));
#23875=CARTESIAN_POINT('Ctrl Pts',(7.87934965382892,2.12005107789844,2.42948400971865));
#23876=CARTESIAN_POINT('Ctrl Pts',(7.87291070021048,2.19642200451226,2.35835704264523));
#23877=CARTESIAN_POINT('Ctrl Pts',(7.86647198425604,2.27279011224884,2.2872327008927));
#23878=CARTESIAN_POINT('Ctrl Pts',(7.8600332683016,2.34570848149363,2.21238837156018));
#23879=CARTESIAN_POINT('Ctrl Pts',(7.85359455234716,2.41482460916936,2.13418360724893));
#23880=CARTESIAN_POINT('Ctrl Pts',(7.84715637966308,2.48393490513216,2.05598544150953));
#23881=CARTESIAN_POINT('Ctrl Pts',(7.84071820697899,2.54924335038943,1.97442769278971));
#23882=CARTESIAN_POINT('Ctrl Pts',(7.8342800342949,2.61043658839468,1.88990433103646));
#23883=CARTESIAN_POINT('Ctrl Pts',(7.82784013254177,2.67164626077324,1.80535826925087));
#23884=CARTESIAN_POINT('Ctrl Pts',(7.82140023078864,2.7287382963448,1.71784531159995));
#23885=CARTESIAN_POINT('Ctrl Pts',(7.81496032903552,2.78144169526556,1.62778980778792));
#23886=CARTESIAN_POINT('Ctrl Pts',(7.81211877573837,2.80469663341757,1.58805356279649));
#23887=CARTESIAN_POINT('Ctrl Pts',(7.80927722244123,2.8270977055468,1.54782266328821));
#23888=CARTESIAN_POINT('Ctrl Pts',(7.80643566914408,2.84862442585766,1.50713517738361));
#23889=CARTESIAN_POINT('Ctrl Pts',(7.99126248314343,-2.84862442585767,1.50713517738358));
#23890=CARTESIAN_POINT('Ctrl Pts',(7.98482163489325,-2.79983057110731,1.59936006109635));
#23891=CARTESIAN_POINT('Ctrl Pts',(7.97838078664307,-2.74654152490177,1.68923725024687));
#23892=CARTESIAN_POINT('Ctrl Pts',(7.97193993839289,-2.68900863044322,1.77633052889993));
#23893=CARTESIAN_POINT('Ctrl Pts',(7.96550056115981,-2.6314888758489,1.8634039164304));
#23894=CARTESIAN_POINT('Ctrl Pts',(7.95906118392673,-2.56972741363481,1.94769434405312));
#23895=CARTESIAN_POINT('Ctrl Pts',(7.95262180669365,-2.50401938198163,2.02879385280032));
#23896=CARTESIAN_POINT('Ctrl Pts',(7.94618300148975,-2.43831718736983,2.10988615723509));
#23897=CARTESIAN_POINT('Ctrl Pts',(7.93974419628585,-2.36866936148764,2.18778781344658));
#23898=CARTESIAN_POINT('Ctrl Pts',(7.93330539108195,-2.29541163192632,2.26212356040012));
#23899=CARTESIAN_POINT('Ctrl Pts',(7.92686625944756,-2.22215018839074,2.33646307598059));
#23900=CARTESIAN_POINT('Ctrl Pts',(7.92042712781316,-2.14527874384496,2.40723605288399));
#23901=CARTESIAN_POINT('Ctrl Pts',(7.91398799617877,-2.06516995593504,2.47410400258422));
#23902=CARTESIAN_POINT('Ctrl Pts',(7.90754548029631,-1.98501906483074,2.54100709642228));
#23903=CARTESIAN_POINT('Ctrl Pts',(7.90110296441384,-1.90162772204247,2.60400081859401));
#23904=CARTESIAN_POINT('Ctrl Pts',(7.89466044853138,-1.81540185713925,2.66278682203352));
#23905=CARTESIAN_POINT('Ctrl Pts',(7.88821639548582,-1.72915541902836,2.72158685162003));
#23906=CARTESIAN_POINT('Ctrl Pts',(7.88177234244027,-1.64007342840465,2.77617695343437));
#23907=CARTESIAN_POINT('Ctrl Pts',(7.87532828939471,-1.54859015386917,2.82630254888599));
#23908=CARTESIAN_POINT('Ctrl Pts',(7.86887942669151,-1.45703859882338,2.87646555665429));
#23909=CARTESIAN_POINT('Ctrl Pts',(7.86243056398832,-1.36308251569372,2.92215722470595));
#23910=CARTESIAN_POINT('Ctrl Pts',(7.85598170128512,-1.267180248423,2.96316921226356));
#23911=CARTESIAN_POINT('Ctrl Pts',(7.85314488273283,-1.22499337865672,2.98121015568635));
#23912=CARTESIAN_POINT('Ctrl Pts',(7.85030806418053,-1.18243017790787,2.99834617116936));
#23913=CARTESIAN_POINT('Ctrl Pts',(7.84747124562824,-1.13953080950289,3.01456250502352));
#23914=CARTESIAN_POINT('Ctrl Pts',(7.84116586093479,-1.04417856334637,3.05060648224064));
#23915=CARTESIAN_POINT('Ctrl Pts',(7.83486047624134,-0.947036625504087,
3.08215183084003));
#23916=CARTESIAN_POINT('Ctrl Pts',(7.82855509154788,-0.848556837951724,
3.10903021137868));
#23917=CARTESIAN_POINT('Ctrl Pts',(7.82225387161886,-0.750142097202377,
3.13589083850043));
#23918=CARTESIAN_POINT('Ctrl Pts',(7.81595265168983,-0.650391658679559,
3.15809052349607));
#23919=CARTESIAN_POINT('Ctrl Pts',(7.80965143176081,-0.549773336716463,
3.17551048506152));
#23920=CARTESIAN_POINT('Ctrl Pts',(7.80335298130107,-0.449199237833256,
3.19292279032405));
#23921=CARTESIAN_POINT('Ctrl Pts',(7.79705453084133,-0.347758417372287,
3.20555948358099));
#23922=CARTESIAN_POINT('Ctrl Pts',(7.79075608038159,-0.245929046638912,
3.2133528387837));
#23923=CARTESIAN_POINT('Ctrl Pts',(7.78445900692879,-0.144121938484396,
3.22114449015398));
#23924=CARTESIAN_POINT('Ctrl Pts',(7.77816193347599,-0.0419268570160417,
3.22409488121527));
#23925=CARTESIAN_POINT('Ctrl Pts',(7.77186486002319,0.0601734193822794,
3.22218818849859));
#23926=CARTESIAN_POINT('Ctrl Pts',(7.76556565740319,0.162308217937866,3.22028085109076));
#23927=CARTESIAN_POINT('Ctrl Pts',(7.75926645478319,0.264347737840848,3.21351315207759));
#23928=CARTESIAN_POINT('Ctrl Pts',(7.75296725216318,0.365809917568325,3.20192140233152));
#23929=CARTESIAN_POINT('Ctrl Pts',(7.74666706300651,0.467287987586547,3.19032783716739));
#23930=CARTESIAN_POINT('Ctrl Pts',(7.74036687384983,0.568188131474593,3.17390877081012));
#23931=CARTESIAN_POINT('Ctrl Pts',(7.73406668469315,0.668035385755841,3.15275217641318));
#23932=CARTESIAN_POINT('Ctrl Pts',(7.72776116694932,0.767967089056463,3.13157768814762));
#23933=CARTESIAN_POINT('Ctrl Pts',(7.7214556492055,0.866843724786049,3.10565776049382));
#23934=CARTESIAN_POINT('Ctrl Pts',(7.71515013146167,0.964202481813624,3.07513107632251));
#23935=CARTESIAN_POINT('Ctrl Pts',(7.71132675701214,1.02323633108352,3.05662110631983));
#23936=CARTESIAN_POINT('Ctrl Pts',(7.7075033825626,1.08171239565747,3.03641836763166));
#23937=CARTESIAN_POINT('Ctrl Pts',(7.70368000811307,1.13953080950288,3.01456250502353));
#23938=CARTESIAN_POINT('Ctrl Pts',(7.6972313981056,1.23704895925796,2.97769979743446));
#23939=CARTESIAN_POINT('Ctrl Pts',(7.69078278809813,1.33282880508769,2.93608147108646));
#23940=CARTESIAN_POINT('Ctrl Pts',(7.68433417809066,1.42640355388129,2.88989454201617));
#23941=CARTESIAN_POINT('Ctrl Pts',(7.67788947854617,1.51992155857184,2.84373562088494));
#23942=CARTESIAN_POINT('Ctrl Pts',(7.67144477900168,1.61123679047021,2.79301378365583));
#23943=CARTESIAN_POINT('Ctrl Pts',(7.66500007945719,1.69990406870537,2.73796342555903));
#23944=CARTESIAN_POINT('Ctrl Pts',(7.65855838592108,1.78852998976323,2.68293874466203));
#23945=CARTESIAN_POINT('Ctrl Pts',(7.65211669238497,1.87451009612947,2.62358976554795));
#23946=CARTESIAN_POINT('Ctrl Pts',(7.64567499884886,1.95742568156753,2.56019574713339));
#23947=CARTESIAN_POINT('Ctrl Pts',(7.63923540961072,2.04031418110074,2.49682243754385));
#23948=CARTESIAN_POINT('Ctrl Pts',(7.63279582037259,2.12013985376864,2.42940695253737));
#23949=CARTESIAN_POINT('Ctrl Pts',(7.62635623113445,2.19651503562203,2.35827039602891));
#23950=CARTESIAN_POINT('Ctrl Pts',(7.61991688413659,2.27288734444354,2.28713651548913));
#23951=CARTESIAN_POINT('Ctrl Pts',(7.61347753713873,2.34580913998748,2.21228209717184));
#23952=CARTESIAN_POINT('Ctrl Pts',(7.60703819014087,2.41492786600483,2.13406676664376));
#23953=CARTESIAN_POINT('Ctrl Pts',(7.60059939046314,2.48404071719197,2.05585808412285));
#23954=CARTESIAN_POINT('Ctrl Pts',(7.59416059078541,2.54935089465948,1.9742893455314));
#23955=CARTESIAN_POINT('Ctrl Pts',(7.58772179110768,2.61054498889689,1.8897545934447));
#23956=CARTESIAN_POINT('Ctrl Pts',(7.5812812743156,2.67175540252035,1.80519729743));
#23957=CARTESIAN_POINT('Ctrl Pts',(7.57484075752352,2.72884731845376,1.7176727159187));
#23958=CARTESIAN_POINT('Ctrl Pts',(7.56840024073143,2.78154968390752,1.62760527108202));
#23959=CARTESIAN_POINT('Ctrl Pts',(7.56556308402025,2.80476596835634,1.58792903642151));
#23960=CARTESIAN_POINT('Ctrl Pts',(7.56272592730906,2.82713101270891,1.54775970968128));
#23961=CARTESIAN_POINT('Ctrl Pts',(7.55988877059788,2.84862442585767,1.5071351773836));
#23962=CARTESIAN_POINT('Origin',(13.3346225254169,0.,0.));
#23963=CARTESIAN_POINT('Ctrl Pts',(8.61626248314343,2.84862442585767,-1.50713517738358));
#23964=CARTESIAN_POINT('Ctrl Pts',(8.60982200511013,2.79983337575478,-1.59935476005409));
#23965=CARTESIAN_POINT('Ctrl Pts',(8.60338152707683,2.74654759928038,-1.68922701463086));
#23966=CARTESIAN_POINT('Ctrl Pts',(8.59694104904353,2.68901838739325,-1.77631575874364));
#23967=CARTESIAN_POINT('Ctrl Pts',(8.59050204743798,2.63150236361482,-1.86338453846292));
#23968=CARTESIAN_POINT('Ctrl Pts',(8.58406304583242,2.56974505211714,-1.94767076278352));
#23969=CARTESIAN_POINT('Ctrl Pts',(8.57762404422686,2.50404154058441,-2.0287665034517));
#23970=CARTESIAN_POINT('Ctrl Pts',(8.57118561840174,2.43834390430984,-2.10985499247685));
#23971=CARTESIAN_POINT('Ctrl Pts',(8.56474719257662,2.36870101076993,-2.18775327209251));
#23972=CARTESIAN_POINT('Ctrl Pts',(8.55830876675151,2.29544853859728,-2.26208611002137));
#23973=CARTESIAN_POINT('Ctrl Pts',(8.55187001659225,2.22219237634915,-2.33642269244887));
#23974=CARTESIAN_POINT('Ctrl Pts',(8.545431266433,2.14532654054445,-2.40719320604775));
#23975=CARTESIAN_POINT('Ctrl Pts',(8.53899251627374,2.06522364102136,-2.47405918988744));
#23976=CARTESIAN_POINT('Ctrl Pts',(8.53255038091548,1.98507862707395,-2.54096032878934));
#23977=CARTESIAN_POINT('Ctrl Pts',(8.52610824555721,1.90169344028278,-2.60395259253624));
#23978=CARTESIAN_POINT('Ctrl Pts',(8.51966611019894,1.81547396325931,-2.66273766098494));
#23979=CARTESIAN_POINT('Ctrl Pts',(8.51322243636635,1.72923389578805,-2.72153676815117));
#23980=CARTESIAN_POINT('Ctrl Pts',(8.50677876253376,1.64015850663556,-2.77612646935679));
#23981=CARTESIAN_POINT('Ctrl Pts',(8.50033508870116,1.548682017426,-2.82625221298478));
#23982=CARTESIAN_POINT('Ctrl Pts',(8.49388659938907,1.45713716610344,-2.87641541653039));
#23983=CARTESIAN_POINT('Ctrl Pts',(8.48743811007697,1.36318796635332,-2.92210782147296));
#23984=CARTESIAN_POINT('Ctrl Pts',(8.48098962076488,1.26729271492413,-2.96312111416328));
#23985=CARTESIAN_POINT('Ctrl Pts',(8.478150162386,1.22506723202623,-2.98118046604224));
#23986=CARTESIAN_POINT('Ctrl Pts',(8.47531070400712,1.18246469931592,-2.99833320990822));
#23987=CARTESIAN_POINT('Ctrl Pts',(8.47247124562825,1.13952539547046,-3.01456455156925));
#23988=CARTESIAN_POINT('Ctrl Pts',(8.46616526790204,1.04416414783162,-3.05061173568797));
#23989=CARTESIAN_POINT('Ctrl Pts',(8.45985929017584,0.947013057033462,-3.08215937900991));
#23990=CARTESIAN_POINT('Ctrl Pts',(8.45355331244963,0.84852405863481,-3.10903915774921));
#23991=CARTESIAN_POINT('Ctrl Pts',(8.44725149488684,0.750100035145118,-3.13590120342994));
#23992=CARTESIAN_POINT('Ctrl Pts',(8.44094967732406,0.650340253866413,-3.15810140435334));
#23993=CARTESIAN_POINT('Ctrl Pts',(8.43464785976127,0.549712617121871,-3.1755209967936));
#23994=CARTESIAN_POINT('Ctrl Pts',(8.42834880851157,0.449129152958476,-3.19293294254369));
#23995=CARTESIAN_POINT('Ctrl Pts',(8.42204975726187,0.347678994127284,-3.20556838689609));
#23996=CARTESIAN_POINT('Ctrl Pts',(8.41575070601216,0.245840395475785,-3.2133596223349));
#23997=CARTESIAN_POINT('Ctrl Pts',(8.40945303005588,0.144024031594194,-3.22114915668661));
#23998=CARTESIAN_POINT('Ctrl Pts',(8.4031553540996,0.0418198044672765,-3.22409655745443));
#23999=CARTESIAN_POINT('Ctrl Pts',(8.39685767814332,-0.0602894271516658,
-3.22218601999849));
#24000=CARTESIAN_POINT('Ctrl Pts',(8.39055787471853,-0.162433153110444,
-3.22027483712855));
#24001=CARTESIAN_POINT('Ctrl Pts',(8.38425807129375,-0.264481410019586,
-3.21350244058091));
#24002=CARTESIAN_POINT('Ctrl Pts',(8.37795826786896,-0.36595205823057,-3.20190515999097));
#24003=CARTESIAN_POINT('Ctrl Pts',(8.37165747903621,-0.467438578362893,
-3.19030606536782));
#24004=CARTESIAN_POINT('Ctrl Pts',(8.36535669020346,-0.568346904093618,
-3.17388063783813));
#24005=CARTESIAN_POINT('Ctrl Pts',(8.35905590137072,-0.668201994268032,
-3.15271686920285));
#24006=CARTESIAN_POINT('Ctrl Pts',(8.3527497907158,-0.768141424839589,-3.13153522505768));
#24007=CARTESIAN_POINT('Ctrl Pts',(8.34644368006089,-0.867025443845474,
-3.1056073379909));
#24008=CARTESIAN_POINT('Ctrl Pts',(8.34013756940597,-0.964391162463139,
-3.07507190944586));
#24009=CARTESIAN_POINT('Ctrl Pts',(8.33631838230833,-1.02335902976613,-3.05657865407787));
#24010=CARTESIAN_POINT('Ctrl Pts',(8.33249919521069,-1.08177028398587,-3.03639636678802));
#24011=CARTESIAN_POINT('Ctrl Pts',(8.32868000811305,-1.13952539547056,-3.01456455156921));
#24012=CARTESIAN_POINT('Ctrl Pts',(8.32223177201094,-1.23703792508388,-2.97770416859512));
#24013=CARTESIAN_POINT('Ctrl Pts',(8.31578353590882,-1.3328124689087,-2.93608867740333));
#24014=CARTESIAN_POINT('Ctrl Pts',(8.3093352998067,-1.42638227424303,-2.88990504519185));
#24015=CARTESIAN_POINT('Ctrl Pts',(8.30289097828219,-1.51989527547491,-2.84374945001395));
#24016=CARTESIAN_POINT('Ctrl Pts',(8.29644665675767,-1.611205864902,-2.7930314060247));
#24017=CARTESIAN_POINT('Ctrl Pts',(8.29000233523316,-1.69986889868451,-2.7379852610606));
#24018=CARTESIAN_POINT('Ctrl Pts',(8.28356102216947,-1.78849054110208,-2.68296481378559));
#24019=CARTESIAN_POINT('Ctrl Pts',(8.27711970910578,-1.8744667685495,-2.62362049134033));
#24020=CARTESIAN_POINT('Ctrl Pts',(8.2706783960421,-1.95737890937776,-2.56023150664606));
#24021=CARTESIAN_POINT('Ctrl Pts',(8.26423918807191,-2.04026395358663,-2.49686323818434));
#24022=CARTESIAN_POINT('Ctrl Pts',(8.25779998010172,-2.12008660575422,-2.4294531723003));
#24023=CARTESIAN_POINT('Ctrl Pts',(8.25136077213152,-2.19645923493826,-2.35832236807321));
#24024=CARTESIAN_POINT('Ctrl Pts',(8.24492180366115,-2.27282902351977,-2.28719420948427));
#24025=CARTESIAN_POINT('Ctrl Pts',(8.23848283519077,-2.34574876363202,-2.21234584315096));
#24026=CARTESIAN_POINT('Ctrl Pts',(8.23204386672039,-2.41486593091617,-2.1341368508604));
#24027=CARTESIAN_POINT('Ctrl Pts',(8.22560544314274,-2.48397724921349,-2.05593447694535));
#24028=CARTESIAN_POINT('Ctrl Pts',(8.21916701956509,-2.54928638752638,-1.97437233073066));
#24029=CARTESIAN_POINT('Ctrl Pts',(8.21272859598744,-2.61047996810889,-1.88984441121544));
#24030=CARTESIAN_POINT('Ctrl Pts',(8.2062884481267,-2.67168993702854,-1.80529385416162));
#24031=CARTESIAN_POINT('Ctrl Pts',(8.19984830026596,-2.72878192470561,-1.71777624531121));
#24032=CARTESIAN_POINT('Ctrl Pts',(8.19340815240522,-2.78148491010336,-1.62771596335704));
#24033=CARTESIAN_POINT('Ctrl Pts',(8.19056835846944,-2.8047243793774,-1.58800373188684));
#24034=CARTESIAN_POINT('Ctrl Pts',(8.18772856453366,-2.82711103391902,-1.54779747143598));
#24035=CARTESIAN_POINT('Ctrl Pts',(8.18488877059788,-2.84862442585766,-1.50713517738361));
#24036=CARTESIAN_POINT('Ctrl Pts',(8.86280938168963,2.84862442585767,-1.50713517738358));
#24037=CARTESIAN_POINT('Ctrl Pts',(8.85636948091779,2.79983774890731,-1.59934649439264));
#24038=CARTESIAN_POINT('Ctrl Pts',(8.84992958014595,2.74655707058332,-1.68921105493153));
#24039=CARTESIAN_POINT('Ctrl Pts',(8.84348967937412,2.68903360032897,-1.77629272891656));
#24040=CARTESIAN_POINT('Ctrl Pts',(8.83705126347726,2.63152339350284,-1.86335432411414));
#24041=CARTESIAN_POINT('Ctrl Pts',(8.8306128475804,2.56977255346136,-1.94763399480922));
#24042=CARTESIAN_POINT('Ctrl Pts',(8.82417443168354,2.50407608910275,-2.02872386057933));
#24043=CARTESIAN_POINT('Ctrl Pts',(8.81773659743177,2.43838555974841,-2.10980640070863));
#24044=CARTESIAN_POINT('Ctrl Pts',(8.81129876318,2.36875035603891,-2.18769941576884));
#24045=CARTESIAN_POINT('Ctrl Pts',(8.80486092892823,2.29550608022533,-2.26202771825382));
#24046=CARTESIAN_POINT('Ctrl Pts',(8.79842277363146,2.22225815183108,-2.33635972737822));
#24047=CARTESIAN_POINT('Ctrl Pts',(8.79198461833468,2.14540106018473,-2.40712640035833));
#24048=CARTESIAN_POINT('Ctrl Pts',(8.78554646303791,2.06530734054498,-2.47398931921523));
#24049=CARTESIAN_POINT('Ctrl Pts',(8.77910492109857,1.98517148945806,-2.54088740976282));
#24050=CARTESIAN_POINT('Ctrl Pts',(8.77266337915924,1.9017959000354,-2.60387739938502));
#24051=CARTESIAN_POINT('Ctrl Pts',(8.76622183721991,1.81558638164062,-2.66266100983605));
#24052=CARTESIAN_POINT('Ctrl Pts',(8.75977875478887,1.72935624628037,-2.72145867835966));
#24053=CARTESIAN_POINT('Ctrl Pts',(8.75333567235783,1.64029114888392,-2.77604775455572));
#24054=CARTESIAN_POINT('Ctrl Pts',(8.7468925899268,1.54882523780716,-2.82617372877741));
#24055=CARTESIAN_POINT('Ctrl Pts',(8.7404446829822,1.45729083800118,-2.87633723681071));
#24056=CARTESIAN_POINT('Ctrl Pts',(8.73399677603761,1.36335236963033,-2.92203078994484));
#24057=CARTESIAN_POINT('Ctrl Pts',(8.72754886909302,1.26746805584356,-2.963046116738));
#24058=CARTESIAN_POINT('Ctrl Pts',(8.72470529412016,1.22518235952123,-2.98113418124867));
#24059=CARTESIAN_POINT('Ctrl Pts',(8.72186171914731,1.18251849092217,-2.99831301466322));
#24060=CARTESIAN_POINT('Ctrl Pts',(8.71901814417445,1.1395169090585,-3.01456775947561));
#24061=CARTESIAN_POINT('Ctrl Pts',(8.71271123131444,1.04414146362609,-3.05062000359505));
#24062=CARTESIAN_POINT('Ctrl Pts',(8.70640431845443,0.946975935947859,-3.08217126797956));
#24063=CARTESIAN_POINT('Ctrl Pts',(8.70009740559442,0.848472409229412,-3.10905325352855));
#24064=CARTESIAN_POINT('Ctrl Pts',(8.69379464562084,0.75003374371466,-3.13591753820937));
#24065=CARTESIAN_POINT('Ctrl Pts',(8.68749188564727,0.650259225611314,-3.158118554212));
#24066=CARTESIAN_POINT('Ctrl Pts',(8.68118912567369,0.54961689606934,-3.17553756552416));
#24067=CARTESIAN_POINT('Ctrl Pts',(8.67488912702297,0.449018659268668,-3.1929489453361));
#24068=CARTESIAN_POINT('Ctrl Pts',(8.66858912837225,0.347553770145556,-3.20558242067925));
#24069=CARTESIAN_POINT('Ctrl Pts',(8.66228912972153,0.245700615361503,-3.21337031325538));
#24070=CARTESIAN_POINT('Ctrl Pts',(8.65599050365746,0.143869651420295,-3.22115650907601));
#24071=CARTESIAN_POINT('Ctrl Pts',(8.64969187759338,0.0416509977878185,
-3.22409919364228));
#24072=CARTESIAN_POINT('Ctrl Pts',(8.64339325152931,-0.060472359969582,
-3.22218259199874));
#24073=CARTESIAN_POINT('Ctrl Pts',(8.63709250068388,-0.162630168066401,
-3.22026534380794));
#24074=CARTESIAN_POINT('Ctrl Pts',(8.63079174983846,-0.264692206811846,
-3.21348553770968));
#24075=CARTESIAN_POINT('Ctrl Pts',(8.62449099899304,-0.366176213280718,
-3.20187953291928));
#24076=CARTESIAN_POINT('Ctrl Pts',(8.61818926453202,-0.467676062504604,
-3.19027171630556));
#24077=CARTESIAN_POINT('Ctrl Pts',(8.61188753007099,-0.56859729414741,-3.17383625467164));
#24078=CARTESIAN_POINT('Ctrl Pts',(8.60558579560997,-0.668464744479618,
-3.15266116921686));
#24079=CARTESIAN_POINT('Ctrl Pts',(8.59927875002009,-0.768416363527621,
-3.13146823730916));
#24080=CARTESIAN_POINT('Ctrl Pts',(8.59297170443021,-0.867312028348975,
-3.10552779483726));
#24081=CARTESIAN_POINT('Ctrl Pts',(8.58666465884034,-0.964688727521637,
-3.07497857252578));
#24082=CARTESIAN_POINT('Ctrl Pts',(8.58285207477998,-1.02355255620746,-3.05651168872394));
#24083=CARTESIAN_POINT('Ctrl Pts',(8.57903949071962,-1.08186161698839,-3.03636165679441));
#24084=CARTESIAN_POINT('Ctrl Pts',(8.57522690665926,-1.13951690905862,-3.01456775947556));
#24085=CARTESIAN_POINT('Ctrl Pts',(8.56877925371523,-1.23702067757096,-2.97771100196281));
#24086=CARTESIAN_POINT('Ctrl Pts',(8.56233160077121,-1.33278695607169,-2.93609993215246));
#24087=CARTESIAN_POINT('Ctrl Pts',(8.55588394782718,-1.42634905487053,-2.8899214411762));
#24088=CARTESIAN_POINT('Ctrl Pts',(8.54944021584167,-1.51985425651467,-2.84377103234837));
#24089=CARTESIAN_POINT('Ctrl Pts',(8.54299648385614,-1.61115760892541,-2.79305890321962));
#24090=CARTESIAN_POINT('Ctrl Pts',(8.53655275187063,-1.69981402601576,-2.73801932780982));
#24091=CARTESIAN_POINT('Ctrl Pts',(8.53011203214013,-1.78842899884087,-2.68300548178134));
#24092=CARTESIAN_POINT('Ctrl Pts',(8.52367131240963,-1.87439917965038,-2.62366842015394));
#24093=CARTESIAN_POINT('Ctrl Pts',(8.51723059267913,-1.9573059507449,-2.56028728420828));
#24094=CARTESIAN_POINT('Ctrl Pts',(8.51079197925771,-2.04018560883168,-2.49692687580039));
#24095=CARTESIAN_POINT('Ctrl Pts',(8.50435336583628,-2.12000355256081,-2.4295252593403));
#24096=CARTESIAN_POINT('Ctrl Pts',(8.49791475241485,-2.19637220248192,-2.35840342406992));
#24097=CARTESIAN_POINT('Ctrl Pts',(8.4914763741916,-2.27273806270812,-2.28728418683188));
#24098=CARTESIAN_POINT('Ctrl Pts',(8.48503799596835,-2.34565459889792,-2.21244525647574));
#24099=CARTESIAN_POINT('Ctrl Pts',(8.4785996177451,-2.41476933644808,-2.13424614659371));
#24100=CARTESIAN_POINT('Ctrl Pts',(8.472161780618,-2.48387826543627,-2.05605360874526));
#24101=CARTESIAN_POINT('Ctrl Pts',(8.46572394349091,-2.5491857839952,-1.97450174114556));
#24102=CARTESIAN_POINT('Ctrl Pts',(8.45928610636381,-2.61037856394492,-1.88998447490894));
#24103=CARTESIAN_POINT('Ctrl Pts',(8.45284653376126,-2.67158783989571,-1.80544442498911));
#24104=CARTESIAN_POINT('Ctrl Pts',(8.4464069611587,-2.72867993959428,-1.71793768779669));
#24105=CARTESIAN_POINT('Ctrl Pts',(8.43996738855614,-2.78138389155642,-1.62788857428586));
#24106=CARTESIAN_POINT('Ctrl Pts',(8.43712348208546,-2.80465952167455,-1.58812021194276));
#24107=CARTESIAN_POINT('Ctrl Pts',(8.43427957561477,-2.82707987863898,-1.54785635778742));
#24108=CARTESIAN_POINT('Ctrl Pts',(8.43143566914408,-2.84862442585766,-1.5071351773836));
#24109=CARTESIAN_POINT('Origin',(13.3346225254169,0.,0.));
#24110=CARTESIAN_POINT('Ctrl Pts',(9.48780938168963,-2.84862442585767,1.50713517738359));
#24111=CARTESIAN_POINT('Ctrl Pts',(9.48136979040113,-2.79984009345644,1.59934206297865));
#24112=CARTESIAN_POINT('Ctrl Pts',(9.47493019911264,-2.74656214827031,1.68920249868086));
#24113=CARTESIAN_POINT('Ctrl Pts',(9.46849060782414,-2.68904175600906,1.77628038241144));
#24114=CARTESIAN_POINT('Ctrl Pts',(9.46205250594599,-2.63153466761499,1.86333812593513));
#24115=CARTESIAN_POINT('Ctrl Pts',(9.45561440406783,-2.56978729677783,1.94761428328878));
#24116=CARTESIAN_POINT('Ctrl Pts',(9.44917630218968,-2.50409461012863,2.02870099966081));
#24117=CARTESIAN_POINT('Ctrl Pts',(9.44273878510985,-2.43840789060658,2.10978035060493));
#24118=CARTESIAN_POINT('Ctrl Pts',(9.43630126803001,-2.36877680910113,2.18767054344086));
#24119=CARTESIAN_POINT('Ctrl Pts',(9.42986375095017,-2.29553692688901,2.26199641462779));
#24120=CARTESIAN_POINT('Ctrl Pts',(9.42342591460022,-2.22229341232837,2.33632597202311));
#24121=CARTESIAN_POINT('Ctrl Pts',(9.41698807825027,-2.14544100795,2.40709058612817));
#24122=CARTESIAN_POINT('Ctrl Pts',(9.41055024190032,-2.06535220900859,2.47395186194949));
#24123=CARTESIAN_POINT('Ctrl Pts',(9.40410901815544,-1.98522126976148,2.54084831815358));
#24124=CARTESIAN_POINT('Ctrl Pts',(9.39766779441055,-1.90185082497803,2.60383708854403));
#24125=CARTESIAN_POINT('Ctrl Pts',(9.39122657066567,-1.815646644735,2.66261991729246));
#24126=CARTESIAN_POINT('Ctrl Pts',(9.38478380536225,-1.72942183350709,2.72141681435694));
#24127=CARTESIAN_POINT('Ctrl Pts',(9.37834104005883,-1.64036225290246,2.77600555530531));
#24128=CARTESIAN_POINT('Ctrl Pts',(9.37189827475541,-1.54890201198458,2.82613165294367));
#24129=CARTESIAN_POINT('Ctrl Pts',(9.36545068011865,-1.45737321479151,2.87629532383254));
#24130=CARTESIAN_POINT('Ctrl Pts',(9.35900308548189,-1.36344049892566,2.9219894921406));
#24131=CARTESIAN_POINT('Ctrl Pts',(9.35255549084513,-1.26756204807032,2.96300590900386));
#24132=CARTESIAN_POINT('Ctrl Pts',(9.34970970862157,-1.22524406649145,2.98110937185465));
#24133=CARTESIAN_POINT('Ctrl Pts',(9.34686392639801,-1.18254731002768,2.99830219557313));
#24134=CARTESIAN_POINT('Ctrl Pts',(9.34401814417445,-1.13951233461232,3.01456948862792));
#24135=CARTESIAN_POINT('Ctrl Pts',(9.33771072418351,-1.04412918758265,3.05062447855748));
#24136=CARTESIAN_POINT('Ctrl Pts',(9.33140330419258,-0.946955828523528,
3.08217770810489));
#24137=CARTESIAN_POINT('Ctrl Pts',(9.32509588420165,-0.84844442075252,3.10906089155454));
#24138=CARTESIAN_POINT('Ctrl Pts',(9.31879261313949,-0.7499978123472,3.13592639163863));
#24139=CARTESIAN_POINT('Ctrl Pts',(9.31248934207733,-0.650215299854983,
3.15812785052148));
#24140=CARTESIAN_POINT('Ctrl Pts',(9.30618607101517,-0.549564999754426,
3.17554654721749));
#24141=CARTESIAN_POINT('Ctrl Pts',(9.29988555856276,-0.448958748988868,
3.19295762066742));
#24142=CARTESIAN_POINT('Ctrl Pts',(9.29358504611035,-0.347485868817361,
3.2055900284188));
#24143=CARTESIAN_POINT('Ctrl Pts',(9.28728453365794,-0.245624817427304,
3.21337610801534));
#24144=CARTESIAN_POINT('Ctrl Pts',(9.28098539232177,-0.143785933018701,
3.22116049320681));
#24145=CARTESIAN_POINT('Ctrl Pts',(9.27468625098561,-0.0415594530327246,
3.2241006196819));
#24146=CARTESIAN_POINT('Ctrl Pts',(9.26838710964944,0.0605715681494443,
3.22218072857993));
#24147=CARTESIAN_POINT('Ctrl Pts',(9.26208584499361,0.162737015739041,3.22026019031953));
#24148=CARTESIAN_POINT('Ctrl Pts',(9.25578458033778,0.264806531084418,3.21347636482852));
#24149=CARTESIAN_POINT('Ctrl Pts',(9.24948331568195,0.366297784362431,3.20186562736027));
#24150=CARTESIAN_POINT('Ctrl Pts',(9.243181068389,0.467804864474859,3.19025307928063));
#24151=CARTESIAN_POINT('Ctrl Pts',(9.23687882109605,0.568733097433191,3.17381217428114));
#24152=CARTESIAN_POINT('Ctrl Pts',(9.23057657380311,0.668607252988596,3.15263094950092));
#24153=CARTESIAN_POINT('Ctrl Pts',(9.22426902119375,0.768565483949464,3.13143189408121));
#24154=CARTESIAN_POINT('Ctrl Pts',(9.21796146858439,0.867467466274419,3.10548464033273));
#24155=CARTESIAN_POINT('Ctrl Pts',(9.21165391597503,0.964850122006924,3.07492793485688));
#24156=CARTESIAN_POINT('Ctrl Pts',(9.20784491286977,1.02365753290874,3.0564753601021));
#24157=CARTESIAN_POINT('Ctrl Pts',(9.20403590976451,1.08191117538282,3.03634282365224));
#24158=CARTESIAN_POINT('Ctrl Pts',(9.20022690665925,1.13951233461235,3.01456948862791));
#24159=CARTESIAN_POINT('Ctrl Pts',(9.19377956644096,1.23701140727205,2.97771467525302));
#24160=CARTESIAN_POINT('Ctrl Pts',(9.18733222622268,1.3327732555634,2.93610597621625));
#24161=CARTESIAN_POINT('Ctrl Pts',(9.18088488600439,1.42633122358117,2.88993024191544));
#24162=CARTESIAN_POINT('Ctrl Pts',(9.17444147014678,1.51983224482733,2.843782613815));
#24163=CARTESIAN_POINT('Ctrl Pts',(9.16799805428917,1.61113171828328,2.79307365592956));
#24164=CARTESIAN_POINT('Ctrl Pts',(9.16155463843156,1.69978458883192,2.73803760274937));
#24165=CARTESIAN_POINT('Ctrl Pts',(9.15511423684688,1.78839598697616,2.68302729580209));
#24166=CARTESIAN_POINT('Ctrl Pts',(9.14867383526221,1.8743629269146,2.62369412683514));
#24167=CARTESIAN_POINT('Ctrl Pts',(9.14223343367753,1.95726681988284,2.5603171987638));
#24168=CARTESIAN_POINT('Ctrl Pts',(9.13579513903988,2.0401435912332,2.4969610041558));
#24169=CARTESIAN_POINT('Ctrl Pts',(9.12935684440223,2.11995901137559,2.42956391746386));
#24170=CARTESIAN_POINT('Ctrl Pts',(9.12291854976458,2.19632552848083,2.35844689052846));
#24171=CARTESIAN_POINT('Ctrl Pts',(9.11648048800268,2.27268928337791,2.28733243592503));
#24172=CARTESIAN_POINT('Ctrl Pts',(9.11004242624078,2.34560410244999,2.2124985641213));
#24173=CARTESIAN_POINT('Ctrl Pts',(9.10360436447888,2.41471753778688,2.13430475218617));
#24174=CARTESIAN_POINT('Ctrl Pts',(9.09716684177078,2.48382518631067,2.05611748735687));
#24175=CARTESIAN_POINT('Ctrl Pts',(9.09072931906268,2.54913183681801,1.97457113008197));
#24176=CARTESIAN_POINT('Ctrl Pts',(9.08429179635459,2.61032418772396,1.89005957511482));
#24177=CARTESIAN_POINT('Ctrl Pts',(9.07785253216167,2.67153309244341,1.80552515800072));
#24178=CARTESIAN_POINT('Ctrl Pts',(9.07141326796875,2.72862525233257,1.71802424911479));
#24179=CARTESIAN_POINT('Ctrl Pts',(9.06497400377584,2.78132972249762,1.627981123125));
#24180=CARTESIAN_POINT('Ctrl Pts',(9.06212789223192,2.80462474448441,1.58818266593297));
#24181=CARTESIAN_POINT('Ctrl Pts',(9.059281780688,2.82706317369287,1.54788793167558));
#24182=CARTESIAN_POINT('Ctrl Pts',(9.05643566914408,2.84862442585766,1.50713517738361));
#24183=CARTESIAN_POINT('Ctrl Pts',(9.24126248314343,-2.84862442585767,1.50713517738359));
#24184=CARTESIAN_POINT('Ctrl Pts',(9.23482235122126,-2.79983599778463,1.59934980417595));
#24185=CARTESIAN_POINT('Ctrl Pts',(9.2283822192991,-2.74655327805828,1.68921744557311));
#24186=CARTESIAN_POINT('Ctrl Pts',(9.22194208737694,-2.68902750877139,1.77630195056211));
#24187=CARTESIAN_POINT('Ctrl Pts',(9.2155034369455,-2.63151497273731,1.86336642259395));
#24188=CARTESIAN_POINT('Ctrl Pts',(9.20906478651407,-2.56976154144227,1.94764871747033));
#24189=CARTESIAN_POINT('Ctrl Pts',(9.20262613608263,-2.50406225534015,2.02874093562506));
#24190=CARTESIAN_POINT('Ctrl Pts',(9.19618806494546,-2.43836888029341,2.10982585780106));
#24191=CARTESIAN_POINT('Ctrl Pts',(9.18974999380828,-2.36873059751867,2.18772098086146));
#24192=CARTESIAN_POINT('Ctrl Pts',(9.18331192267111,-2.29548303985887,2.2620510993831));
#24193=CARTESIAN_POINT('Ctrl Pts',(9.17687352916871,-2.22223181456864,2.33638493974084));
#24194=CARTESIAN_POINT('Ctrl Pts',(9.1704351356663,-2.14537122172991,2.40715315055674));
#24195=CARTESIAN_POINT('Ctrl Pts',(9.1639967421639,-2.06527382647043,2.47401729666471));
#24196=CARTESIAN_POINT('Ctrl Pts',(9.15755496259094,-1.98513430650513,2.54091660786734));
#24197=CARTESIAN_POINT('Ctrl Pts',(9.15111318301797,-1.90175487425804,2.60390750811563));
#24198=CARTESIAN_POINT('Ctrl Pts',(9.14467140344501,-1.81554136842773,2.66269170239958));
#24199=CARTESIAN_POINT('Ctrl Pts',(9.138228084184,-1.7293072561948,2.72148994704331));
#24200=CARTESIAN_POINT('Ctrl Pts',(9.131784764923,-1.64023803795771,2.77607927355949));
#24201=CARTESIAN_POINT('Ctrl Pts',(9.125341445662,-1.54876789141397,2.82620515550891));
#24202=CARTESIAN_POINT('Ctrl Pts',(9.11889330549825,-1.45722930674659,2.87636854173088));
#24203=CARTESIAN_POINT('Ctrl Pts',(9.11244516533451,-1.3632865414915,2.92206163521662));
#24204=CARTESIAN_POINT('Ctrl Pts',(9.10599702517076,-1.26739784827073,2.96307614763757));
#24205=CARTESIAN_POINT('Ctrl Pts',(9.1031550986566,-1.22513626388314,2.98115271349298));
#24206=CARTESIAN_POINT('Ctrl Pts',(9.10031317214242,-1.18249695692235,2.99832109910658));
#24207=CARTESIAN_POINT('Ctrl Pts',(9.09747124562826,-1.1395203141202,3.01456647234845));
#24208=CARTESIAN_POINT('Ctrl Pts',(9.09116470883316,-1.04415057890354,3.05061668110268));
#24209=CARTESIAN_POINT('Ctrl Pts',(9.08485817203806,-0.946990857625094,
3.08216648887611));
#24210=CARTESIAN_POINT('Ctrl Pts',(9.07855163524296,-0.848493174102343,
3.10904758664156));
#24211=CARTESIAN_POINT('Ctrl Pts',(9.07224925426397,-0.750060397559917,
3.13591097058044));
#24212=CARTESIAN_POINT('Ctrl Pts',(9.06594687328498,-0.650291806577286,
3.15811165856173));
#24213=CARTESIAN_POINT('Ctrl Pts',(9.05964449230599,-0.549655386463332,
3.17553090342888));
#24214=CARTESIAN_POINT('Ctrl Pts',(9.05334487465865,-0.449063091229409,
3.19294251068244));
#24215=CARTESIAN_POINT('Ctrl Pts',(9.0470452570113,-0.347604126657197,3.20557677780699));
#24216=CARTESIAN_POINT('Ctrl Pts',(9.04074563936396,-0.245756826387187,
3.21336601475526));
#24217=CARTESIAN_POINT('Ctrl Pts',(9.0344473953925,-0.14393173463654,3.22115355320569));
#24218=CARTESIAN_POINT('Ctrl Pts',(9.02814915142105,-0.0417188834012557,
3.22409813452873));
#24219=CARTESIAN_POINT('Ctrl Pts',(9.02185090744959,0.0603987927624763,
3.22218397183228));
#24220=CARTESIAN_POINT('Ctrl Pts',(9.01555053761488,0.162550936980487,3.22026916304333));
#24221=CARTESIAN_POINT('Ctrl Pts',(9.00925016778017,0.264607432624234,3.21349233702463));
#24222=CARTESIAN_POINT('Ctrl Pts',(9.00294979794547,0.366086066356794,3.20188984109688));
#24223=CARTESIAN_POINT('Ctrl Pts',(8.99664844377251,0.46758055460317,3.19028553245325));
#24224=CARTESIAN_POINT('Ctrl Pts',(8.99034708959955,0.568496595473008,3.17385410654971));
#24225=CARTESIAN_POINT('Ctrl Pts',(8.9840457354266,0.668359074543371,3.15268357276393));
#24226=CARTESIAN_POINT('Ctrl Pts',(8.97773906582064,0.768305791430331,3.13149518082403));
#24227=CARTESIAN_POINT('Ctrl Pts',(8.97143239621467,0.867196772356202,3.10555978819097));
#24228=CARTESIAN_POINT('Ctrl Pts',(8.96512572660871,0.964569055215959,3.07501611381466));
#24229=CARTESIAN_POINT('Ctrl Pts',(8.96131048711016,1.02347472220693,3.0565386224932));
#24230=CARTESIAN_POINT('Ctrl Pts',(8.95749524761161,1.08182487959139,3.03637561813463));
#24231=CARTESIAN_POINT('Ctrl Pts',(8.95368000811306,1.1395203141202,3.01456647234845));
#24232=CARTESIAN_POINT('Ctrl Pts',(8.947232121635,1.23702759047468,2.97770826298414));
#24233=CARTESIAN_POINT('Ctrl Pts',(8.94078423515694,1.33279717833878,2.93609542263685));
#24234=CARTESIAN_POINT('Ctrl Pts',(8.93433634867889,1.42636236278996,2.88991487288402));
#24235=CARTESIAN_POINT('Ctrl Pts',(8.92789238060956,1.51987068727056,2.84376238725264));
#24236=CARTESIAN_POINT('Ctrl Pts',(8.92144841254023,1.61117693729572,2.79304788962198));
#24237=CARTESIAN_POINT('Ctrl Pts',(8.9150044444709,1.69983600365082,2.73800568355736));
#24238=CARTESIAN_POINT('Ctrl Pts',(8.90856348714187,1.78845364686092,2.68298919422287));
#24239=CARTESIAN_POINT('Ctrl Pts',(8.90212252981284,1.87442624865628,2.62364922518965));
#24240=CARTESIAN_POINT('Ctrl Pts',(8.89568157248381,1.95733516973162,2.5602649464131));
#24241=CARTESIAN_POINT('Ctrl Pts',(8.88924272098093,2.04021698431255,2.49690139068512));
#24242=CARTESIAN_POINT('Ctrl Pts',(8.88280386947804,2.12003681322233,2.42949639090833));
#24243=CARTESIAN_POINT('Ctrl Pts',(8.87636501797516,2.19640705638776,2.35837096427811));
#24244=CARTESIAN_POINT('Ctrl Pts',(8.86992640339741,2.27277448941996,2.28724815479191));
#24245=CARTESIAN_POINT('Ctrl Pts',(8.86348778881967,2.34569230838318,2.21240544611426));
#24246=CARTESIAN_POINT('Ctrl Pts',(8.85704917424192,2.41480801874585,2.13420237913388));
#24247=CARTESIAN_POINT('Ctrl Pts',(8.85061110228246,2.4839179043387,2.056005902766));
#24248=CARTESIAN_POINT('Ctrl Pts',(8.844173030323,2.54922607139876,1.97444991942677));
#24249=CARTESIAN_POINT('Ctrl Pts',(8.83773495836353,2.61041917189268,1.88992838740391));
#24250=CARTESIAN_POINT('Ctrl Pts',(8.83129515541268,2.67162872525172,1.80538413024774));
#24251=CARTESIAN_POINT('Ctrl Pts',(8.82485535246184,2.72872078006262,1.71787303983451));
#24252=CARTESIAN_POINT('Ctrl Pts',(8.81841554951099,2.78142434499242,1.62781945423424));
#24253=CARTESIAN_POINT('Ctrl Pts',(8.81557328987329,2.80468549389814,1.58807356860144));
#24254=CARTESIAN_POINT('Ctrl Pts',(8.81273103023558,2.82709235453134,1.54783277720073));
#24255=CARTESIAN_POINT('Ctrl Pts',(8.80988877059788,2.84862442585767,1.50713517738359));
#24256=CARTESIAN_POINT('Origin',(13.3346225254169,0.,0.));
#24257=CARTESIAN_POINT('Ctrl Pts',(9.86626248314343,2.84862442585767,-1.50713517738359));
#24258=CARTESIAN_POINT('Ctrl Pts',(9.85982267522957,2.79983845237032,-1.59934516478271));
#24259=CARTESIAN_POINT('Ctrl Pts',(9.8533828673157,2.74655859410983,-1.68920848768861));
#24260=CARTESIAN_POINT('Ctrl Pts',(9.84694305940184,2.68903604740003,-1.77628902442232));
#24261=CARTESIAN_POINT('Ctrl Pts',(9.84050473772321,2.63152677624702,-1.86334946394761));
#24262=CARTESIAN_POINT('Ctrl Pts',(9.83406641604458,2.5697769771344,-1.94762808047689));
#24263=CARTESIAN_POINT('Ctrl Pts',(9.82762809436595,2.50408164628066,-2.02871700127454));
#24264=CARTESIAN_POINT('Ctrl Pts',(9.8211903552778,2.43839226006218,-2.10979858450265));
#24265=CARTESIAN_POINT('Ctrl Pts',(9.81475261618964,2.36875829322387,-2.18769075275974));
#24266=CARTESIAN_POINT('Ctrl Pts',(9.80831487710149,2.29551533572473,-2.26201832573315));
#24267=CARTESIAN_POINT('Ctrl Pts',(9.80187681749998,2.22226873170531,-2.33634959922618));
#24268=CARTESIAN_POINT('Ctrl Pts',(9.79543875789847,2.14541304648722,-2.40711565444394));
#24269=CARTESIAN_POINT('Ctrl Pts',(9.78900069829696,2.06532080332786,-2.47397808030733));
#24270=CARTESIAN_POINT('Ctrl Pts',(9.78255925182548,1.98518642604269,-2.54087568048664));
#24271=CARTESIAN_POINT('Ctrl Pts',(9.776117805354,1.90181238028295,-2.60386530428902));
#24272=CARTESIAN_POINT('Ctrl Pts',(9.76967635888252,1.81560446362589,-2.6626486801983));
#24273=CARTESIAN_POINT('Ctrl Pts',(9.76323337159812,1.72937592578187,-2.72144611726382));
#24274=CARTESIAN_POINT('Ctrl Pts',(9.75679038431372,1.64031248371951,-2.77603509288299));
#24275=CARTESIAN_POINT('Ctrl Pts',(9.75034739702932,1.54884827400627,-2.82616110414955));
#24276=CARTESIAN_POINT('Ctrl Pts',(9.74389958378342,1.45731555527158,-2.87632466107459));
#24277=CARTESIAN_POINT('Ctrl Pts',(9.73745177053753,1.36337881295747,-2.92201839881558));
#24278=CARTESIAN_POINT('Ctrl Pts',(9.73100395729163,1.26749625837215,-2.96303405270891));
#24279=CARTESIAN_POINT('Ctrl Pts',(9.72815972007051,1.22520087539378,-2.98112673700408));
#24280=CARTESIAN_POINT('Ctrl Pts',(9.72531548284938,1.18252713939225,-2.99830976786173));
#24281=CARTESIAN_POINT('Ctrl Pts',(9.72247124562825,1.13951553844249,-3.01456827757278));
#24282=CARTESIAN_POINT('Ctrl Pts',(9.71616418105511,1.04413778915726,-3.05062134299537));
#24283=CARTESIAN_POINT('Ctrl Pts',(9.70985711648197,0.94696991880963,-3.08217319516756));
#24284=CARTESIAN_POINT('Ctrl Pts',(9.70355005190883,0.84846403456833,-3.10905553899316));
#24285=CARTESIAN_POINT('Ctrl Pts',(9.69724713903899,0.750022993044205,-3.1359201871833));
#24286=CARTESIAN_POINT('Ctrl Pts',(9.69094422616915,0.650246083531913,-3.15812133561167));
#24287=CARTESIAN_POINT('Ctrl Pts',(9.68464131329931,0.54960136971356,-3.17554025276156));
#24288=CARTESIAN_POINT('Ctrl Pts',(9.67834116094118,0.449000735659186,-3.19295154087931));
#24289=CARTESIAN_POINT('Ctrl Pts',(9.67204100858305,0.347533456141694,-3.20558469682421));
#24290=CARTESIAN_POINT('Ctrl Pts',(9.66574085622492,0.245677939217087,-3.21337204703751));
#24291=CARTESIAN_POINT('Ctrl Pts',(9.65944207601374,0.143844605999829,-3.22115770119838));
#24292=CARTESIAN_POINT('Ctrl Pts',(9.65314329580256,0.041623611246871,-3.2240996205201));
#24293=CARTESIAN_POINT('Ctrl Pts',(9.64684451559137,-0.0605020388920546,
-3.22218203486239));
#24294=CARTESIAN_POINT('Ctrl Pts',(9.64054361103579,-0.162662132216087,
-3.22026380247432));
#24295=CARTESIAN_POINT('Ctrl Pts',(9.63424270648021,-0.264726407460492,
-3.21348279402017));
#24296=CARTESIAN_POINT('Ctrl Pts',(9.62794180192462,-0.366212581690208,
-3.20187537351343));
#24297=CARTESIAN_POINT('Ctrl Pts',(9.62163991404569,-0.46771459391978,-3.19026614154494));
#24298=CARTESIAN_POINT('Ctrl Pts',(9.61533802616675,-0.5686379198952,-3.17382905160953));
#24299=CARTESIAN_POINT('Ctrl Pts',(9.60903613828781,-0.668507375990506,
-3.15265212967531));
#24300=CARTESIAN_POINT('Ctrl Pts',(9.60272894101787,-0.768460972902217,
-3.13145736601481));
#24301=CARTESIAN_POINT('Ctrl Pts',(9.59642174374794,-0.867358527520858,
-3.10551488606228));
#24302=CARTESIAN_POINT('Ctrl Pts',(9.59011454647801,-0.964737008523535,
-3.07496342529225));
#24303=CARTESIAN_POINT('Ctrl Pts',(9.58630303368969,-1.02358395904113,-3.05650082162806));
#24304=CARTESIAN_POINT('Ctrl Pts',(9.58249152090137,-1.08187644074406,-3.03635602341281));
#24305=CARTESIAN_POINT('Ctrl Pts',(9.57868000811306,-1.13951553844249,-3.01456827757278));
#24306=CARTESIAN_POINT('Ctrl Pts',(9.57223244899357,-1.23701789791085,-2.97771210334857));
#24307=CARTESIAN_POINT('Ctrl Pts',(9.56578488987408,-1.33278284708364,-2.93610174484108));
#24308=CARTESIAN_POINT('Ctrl Pts',(9.55933733075459,-1.42634370640727,-2.88992408095652));
#24309=CARTESIAN_POINT('Ctrl Pts',(9.55289369361583,-1.5198476536684,-2.84377450644728));
#24310=CARTESIAN_POINT('Ctrl Pts',(9.54645005647707,-1.61114984215441,-2.7930633288124));
#24311=CARTESIAN_POINT('Ctrl Pts',(9.54000641933832,-1.69980519506997,-2.73802481020774));
#24312=CARTESIAN_POINT('Ctrl Pts',(9.53356579506128,-1.78841909526034,-2.68301202605128));
#24313=CARTESIAN_POINT('Ctrl Pts',(9.52712517078425,-1.87438830360516,-2.62367613238684));
#24314=CARTESIAN_POINT('Ctrl Pts',(9.52068454650722,-1.95729421108584,-2.56029625898056));
#24315=CARTESIAN_POINT('Ctrl Pts',(9.51424602873174,-2.04017300296176,-2.49693711490045));
#24316=CARTESIAN_POINT('Ctrl Pts',(9.50780751095625,-2.11999018945337,-2.42953685757224));
#24317=CARTESIAN_POINT('Ctrl Pts',(9.50136899318077,-2.1963581993966,-2.35841646501277));
#24318=CARTESIAN_POINT('Ctrl Pts',(9.4949307099079,-2.27272342787692,-2.28729866278837));
#24319=CARTESIAN_POINT('Ctrl Pts',(9.48849242663504,-2.34563944881386,-2.21246125023154));
#24320=CARTESIAN_POINT('Ctrl Pts',(9.48205414336218,-2.41475379561177,-2.13426372997307));
#24321=CARTESIAN_POINT('Ctrl Pts',(9.47561640057324,-2.48386234036715,-2.05607277427549));
#24322=CARTESIAN_POINT('Ctrl Pts',(9.4691786577843,-2.54916959844693,-1.97452256002475));
#24323=CARTESIAN_POINT('Ctrl Pts',(9.46274091499536,-2.61036224964905,-1.89000700742276));
#24324=CARTESIAN_POINT('Ctrl Pts',(9.45630143492861,-2.6715714141911,-1.80546864760419));
#24325=CARTESIAN_POINT('Ctrl Pts',(9.44986195486186,-2.72866353193724,-1.71796365916594));
#24326=CARTESIAN_POINT('Ctrl Pts',(9.44342247479511,-2.78136763937955,-1.62791634217248));
#24327=CARTESIAN_POINT('Ctrl Pts',(9.44057790672937,-2.80464908747939,-1.58813895026034));
#24328=CARTESIAN_POINT('Ctrl Pts',(9.43773333866362,-2.82707486660146,-1.54786583100038));
#24329=CARTESIAN_POINT('Ctrl Pts',(9.43488877059788,-2.84862442585766,-1.5071351773836));
#24330=CARTESIAN_POINT('Ctrl Pts',(10.1128093816896,2.84862442585767,-1.50713517738358));
#24331=CARTESIAN_POINT('Ctrl Pts',(10.1063700807377,2.79984229295584,-1.59933790572201));
#24332=CARTESIAN_POINT('Ctrl Pts',(10.0999307797858,2.74656691174921,-1.68919447186086));
#24333=CARTESIAN_POINT('Ctrl Pts',(10.0934914788339,2.68904940689746,-1.77626879997494));
#24334=CARTESIAN_POINT('Ctrl Pts',(10.0870536715522,2.63154524389488,-1.86332293019352));
#24335=CARTESIAN_POINT('Ctrl Pts',(10.0806158642705,2.56980112743642,-1.94759579171096));
#24336=CARTESIAN_POINT('Ctrl Pts',(10.0741780569888,2.50411198448077,-2.02867955371956));
#24337=CARTESIAN_POINT('Ctrl Pts',(10.0677408374702,2.43842883885472,-2.10975591289073));
#24338=CARTESIAN_POINT('Ctrl Pts',(10.0613036179515,2.3688016241954,-2.18764345826353));
#24339=CARTESIAN_POINT('Ctrl Pts',(10.0548663984329,2.29556586332255,-2.26196704875385));
#24340=CARTESIAN_POINT('Ctrl Pts',(10.0484288613174,2.22232648917418,-2.33629430619057));
#24341=CARTESIAN_POINT('Ctrl Pts',(10.0419913242019,2.14547848162114,-2.40705698892092));
#24342=CARTESIAN_POINT('Ctrl Pts',(10.0355537870864,2.06539429837441,-2.47391672348575));
#24343=CARTESIAN_POINT('Ctrl Pts',(10.0291128618851,1.98526796669807,-2.54081164643239));
#24344=CARTESIAN_POINT('Ctrl Pts',(10.0226719366838,1.90190234777773,-2.6037992730192));
#24345=CARTESIAN_POINT('Ctrl Pts',(10.0162310114826,1.8157031748215,-2.66258136841733));
#24346=CARTESIAN_POINT('Ctrl Pts',(10.0097885437321,1.72948335786382,-2.72137754164965));
#24347=CARTESIAN_POINT('Ctrl Pts',(10.0033460759816,1.64042895216162,-2.77596596799634));
#24348=CARTESIAN_POINT('Ctrl Pts',(9.99690360823108,1.54897402990824,-2.82609218129378));
#24349=CARTESIAN_POINT('Ctrl Pts',(9.99045630664174,1.45745048824178,-2.87625600471926));
#24350=CARTESIAN_POINT('Ctrl Pts',(9.98400900505239,1.36352316841648,-2.92195074989421));
#24351=CARTESIAN_POINT('Ctrl Pts',(9.97756170346304,1.26765021708599,-2.96296818910056));
#24352=CARTESIAN_POINT('Ctrl Pts',(9.97471385036684,1.22530194509901,-2.98108610085371));
#24353=CARTESIAN_POINT('Ctrl Pts',(9.97186599727065,1.18257433236595,-2.99829205143002));
#24354=CARTESIAN_POINT('Ctrl Pts',(9.96901814417446,1.13950802589812,-3.01457111732561));
#24355=CARTESIAN_POINT('Ctrl Pts',(9.96271024438015,1.04411759088132,-3.0506287063043));
#24356=CARTESIAN_POINT('Ctrl Pts',(9.95640234458584,0.946936820960122,-3.08218379611568));
#24357=CARTESIAN_POINT('Ctrl Pts',(9.95009444479154,0.848417955275339,-3.10906811370649));
#24358=CARTESIAN_POINT('Ctrl Pts',(9.94379069017424,0.749963830336331,-3.1359347645209));
#24359=CARTESIAN_POINT('Ctrl Pts',(9.93748693555695,0.650173752527543,-3.15813664302233));
#24360=CARTESIAN_POINT('Ctrl Pts',(9.93118318093965,0.549515909624953,-3.17555504244046));
#24361=CARTESIAN_POINT('Ctrl Pts',(9.92488218236069,0.448902074919152,-3.19296582643265));
#24362=CARTESIAN_POINT('Ctrl Pts',(9.91858118378173,0.347421632456268,-3.20559722429035));
#24363=CARTESIAN_POINT('Ctrl Pts',(9.91228018520277,0.245553108123589,-3.21338158854358));
#24364=CARTESIAN_POINT('Ctrl Pts',(9.90598055634726,0.143706728170867,-3.22116426061641));
#24365=CARTESIAN_POINT('Ctrl Pts',(9.89968092749175,0.04147284167858,-3.22410196655805));
#24366=CARTESIAN_POINT('Ctrl Pts',(9.89338129863624,-0.0606654318365552,
-3.22217896273315));
#24367=CARTESIAN_POINT('Ctrl Pts',(9.88707954784687,-0.162838109070619,
-3.22025531117376));
#24368=CARTESIAN_POINT('Ctrl Pts',(9.8807777970575,-0.264914699921362,-3.21346768213288));
#24369=CARTESIAN_POINT('Ctrl Pts',(9.87447604626814,-0.366412811243082,
-3.2018524660354));
#24370=CARTESIAN_POINT('Ctrl Pts',(9.86817331377162,-0.467926734269368,
-3.19023544048193));
#24371=CARTESIAN_POINT('Ctrl Pts',(9.8618705812751,-0.568861592886876,-3.1737893842466));
#24372=CARTESIAN_POINT('Ctrl Pts',(9.85556784877859,-0.668742093881155,
-3.15260234954735));
#24373=CARTESIAN_POINT('Ctrl Pts',(9.84925981647365,-0.768706581863708,
-3.13139749920623));
#24374=CARTESIAN_POINT('Ctrl Pts',(9.84295178416871,-0.867614542586038,
-3.10544379962069));
#24375=CARTESIAN_POINT('Ctrl Pts',(9.83664375186377,-0.965002835110426,
-3.07488001241168));
#24376=CARTESIAN_POINT('Ctrl Pts',(9.8328381367956,-1.02375687053349,-3.05644098047268));
#24377=CARTESIAN_POINT('Ctrl Pts',(9.82903252172743,-1.08195808238332,-3.03632499871464));
#24378=CARTESIAN_POINT('Ctrl Pts',(9.82522690665926,-1.13950802589812,-3.01457111732561));
#24379=CARTESIAN_POINT('Ctrl Pts',(9.81877985987646,-1.23700269405064,-2.97771812812142));
#24380=CARTESIAN_POINT('Ctrl Pts',(9.81233281309366,-1.33276038693557,-2.93611165344557));
#24381=CARTESIAN_POINT('Ctrl Pts',(9.80588576631086,-1.42631448034508,-2.88993850551494));
#24382=CARTESIAN_POINT('Ctrl Pts',(9.7994426470676,-1.51981158062054,-2.84379348625634));
#24383=CARTESIAN_POINT('Ctrl Pts',(9.79299952782435,-1.61110741578519,-2.79308750353223));
#24384=CARTESIAN_POINT('Ctrl Pts',(9.7865564085811,-1.69975695978144,-2.73805475478022));
#24385=CARTESIAN_POINT('Ctrl Pts',(9.78011630549264,-1.78836500512812,-2.68304776797409));
#24386=CARTESIAN_POINT('Ctrl Pts',(9.77367620240419,-1.8743289053089,-2.62371825083255));
#24387=CARTESIAN_POINT('Ctrl Pts',(9.76723609931573,-1.95723009871279,-2.56034527030882));
#24388=CARTESIAN_POINT('Ctrl Pts',(9.76079810376318,-2.04010416254446,-2.49699302871274));
#24389=CARTESIAN_POINT('Ctrl Pts',(9.75436010821063,-2.11991721573218,-2.42960019145055));
#24390=CARTESIAN_POINT('Ctrl Pts',(9.74792211265809,-2.19628173237039,-2.35848767530299));
#24391=CARTESIAN_POINT('Ctrl Pts',(9.74148434779094,-2.27264351272534,-2.28737770724971));
#24392=CARTESIAN_POINT('Ctrl Pts',(9.7350465829238,-2.34555672132969,-2.21254858085581));
#24393=CARTESIAN_POINT('Ctrl Pts',(9.72860881805666,-2.41466893532812,-2.1343597389525));
#24394=CARTESIAN_POINT('Ctrl Pts',(9.7221715903222,-2.48377538297294,-2.0561774207081));
#24395=CARTESIAN_POINT('Ctrl Pts',(9.71573436258774,-2.54908121938732,-1.97463623267522));
#24396=CARTESIAN_POINT('Ctrl Pts',(9.70929713485327,-2.61027316795172,-1.89013003551906));
#24397=CARTESIAN_POINT('Ctrl Pts',(9.70285815998966,-2.67148172463404,-1.80560090252054));
#24398=CARTESIAN_POINT('Ctrl Pts',(9.69641918512605,-2.72857394111304,-1.71810546120604));
#24399=CARTESIAN_POINT('Ctrl Pts',(9.68998021026243,-2.78127889745783,-1.62806795222305));
#24400=CARTESIAN_POINT('Ctrl Pts',(9.68713202988965,-2.80459211507232,-1.58824126065622));
#24401=CARTESIAN_POINT('Ctrl Pts',(9.68428384951686,-2.82704750089152,-1.54791755471499));
#24402=CARTESIAN_POINT('Ctrl Pts',(9.68143566914408,-2.84862442585766,-1.5071351773836));
#24403=CARTESIAN_POINT('Origin',(13.3346225254169,0.,0.));
#24404=CARTESIAN_POINT('Ctrl Pts',(10.7378093816896,-2.84862442585766,1.5071351773836));
#24405=CARTESIAN_POINT('Ctrl Pts',(10.7313703534291,-2.7998443587803,1.59933400112333));
#24406=CARTESIAN_POINT('Ctrl Pts',(10.7249313251685,-2.74657138566347,1.68918693295203));
#24407=CARTESIAN_POINT('Ctrl Pts',(10.718492296908,-2.68905659259001,1.77625792168486));
#24408=CARTESIAN_POINT('Ctrl Pts',(10.7120547663237,-2.63155517708473,1.86330865826993));
#24409=CARTESIAN_POINT('Ctrl Pts',(10.7056172357394,-2.56981411703793,1.94757842439466));
#24410=CARTESIAN_POINT('Ctrl Pts',(10.6991797051551,-2.50412830212752,2.02865941177516));
#24411=CARTESIAN_POINT('Ctrl Pts',(10.6927427651249,-2.43844851297953,2.10973296109971));
#24412=CARTESIAN_POINT('Ctrl Pts',(10.6863058250947,-2.36882492985391,2.18761802006119));
#24413=CARTESIAN_POINT('Ctrl Pts',(10.6798688850646,-2.29559303943354,2.26193946864285));
#24414=CARTESIAN_POINT('Ctrl Pts',(10.673431629017,-2.22235755374044,2.3362645659884));
#24415=CARTESIAN_POINT('Ctrl Pts',(10.6669943729694,-2.14551367537334,2.40702543484564));
#24416=CARTESIAN_POINT('Ctrl Pts',(10.6605571169217,-2.06543382676692,2.47388372195359));
#24417=CARTESIAN_POINT('Ctrl Pts',(10.6541164721538,-1.98531182227798,2.54077720480862));
#24418=CARTESIAN_POINT('Ctrl Pts',(10.6476758273859,-1.90195073547167,2.60376375711341));
#24419=CARTESIAN_POINT('Ctrl Pts',(10.641235182618,-1.81575626491601,2.66254516373305));
#24420=CARTESIAN_POINT('Ctrl Pts',(10.6347929943798,-1.72954113826053,2.72134065704056));
#24421=CARTESIAN_POINT('Ctrl Pts',(10.6283508061416,-1.64049159241196,2.77592878782993));
#24422=CARTESIAN_POINT('Ctrl Pts',(10.6219086179034,-1.5490416649257,2.82605510965802));
#24423=CARTESIAN_POINT('Ctrl Pts',(10.6154615916098,-1.45752305894043,2.87621907613646));
#24424=CARTESIAN_POINT('Ctrl Pts',(10.6090145653162,-1.36360080667019,2.92191436290365));
#24425=CARTESIAN_POINT('Ctrl Pts',(10.6025675390226,-1.26773301998384,2.96293276206914));
#24426=CARTESIAN_POINT('Ctrl Pts',(10.5997177407399,-1.22535629598354,2.98106424752897));
#24427=CARTESIAN_POINT('Ctrl Pts',(10.5968679424572,-1.18259969928859,2.99828252911706));
#24428=CARTESIAN_POINT('Ctrl Pts',(10.5940181441744,-1.13950396258885,3.01457265325358));
#24429=CARTESIAN_POINT('Ctrl Pts',(10.5877097898818,-1.04410662262551,3.05063270534465));
#24430=CARTESIAN_POINT('Ctrl Pts',(10.5814014355892,-0.946918831284225,
3.08218955825583));
#24431=CARTESIAN_POINT('Ctrl Pts',(10.5750930812966,-0.848392899556238,
3.10907495092713));
#24432=CARTESIAN_POINT('Ctrl Pts',(10.5687888686204,-0.749931652942532,
3.13594269256315));
#24433=CARTESIAN_POINT('Ctrl Pts',(10.5624846559442,-0.650134407193353,
3.1581449691306));
#24434=CARTESIAN_POINT('Ctrl Pts',(10.556180443268,-0.549469417647791,3.17556308732322));
#24435=CARTESIAN_POINT('Ctrl Pts',(10.5498789841903,-0.4488483972663,3.19297359750734));
#24436=CARTESIAN_POINT('Ctrl Pts',(10.5435775251126,-0.347360789604111,
3.20560403890608));
#24437=CARTESIAN_POINT('Ctrl Pts',(10.5372760660349,-0.24548518470401,3.21338677824361));
#24438=CARTESIAN_POINT('Ctrl Pts',(10.5309759753598,-0.14363170275086,3.22116782750892));
#24439=CARTESIAN_POINT('Ctrl Pts',(10.5246758846847,-0.0413907985953394,
3.22410324032225));
#24440=CARTESIAN_POINT('Ctrl Pts',(10.5183757940096,0.0607543465188861,
3.22217728746869));
#24441=CARTESIAN_POINT('Ctrl Pts',(10.512073582716,0.162933873818505,3.22025068633695));
#24442=CARTESIAN_POINT('Ctrl Pts',(10.5057713714224,0.26501716870336,3.21345945366387));
#24443=CARTESIAN_POINT('Ctrl Pts',(10.4994691601288,0.366521778017622,3.20183999424375));
#24444=CARTESIAN_POINT('Ctrl Pts',(10.4931659680128,0.468042184643721,3.19021872647004));
#24445=CARTESIAN_POINT('Ctrl Pts',(10.4868627758968,0.56898332101638,3.17376778957782));
#24446=CARTESIAN_POINT('Ctrl Pts',(10.4805595837808,0.668869834247954,3.1525752500667));
#24447=CARTESIAN_POINT('Ctrl Pts',(10.4742510970817,0.768840250591654,3.13136490915316));
#24448=CARTESIAN_POINT('Ctrl Pts',(10.4679426103827,0.867753875672361,3.10540510221069));
#24449=CARTESIAN_POINT('Ctrl Pts',(10.4616341236837,0.965147508863338,3.07483460508608));
#24450=CARTESIAN_POINT('Ctrl Pts',(10.4578317180089,1.02385098581493,3.05640840601582));
#24451=CARTESIAN_POINT('Ctrl Pts',(10.4540293123341,1.08200253352952,3.0363081075963));
#24452=CARTESIAN_POINT('Ctrl Pts',(10.4502269066593,1.13950396258886,3.01457265325358));
#24453=CARTESIAN_POINT('Ctrl Pts',(10.443780135533,1.23699449471016,2.97772137765163));
#24454=CARTESIAN_POINT('Ctrl Pts',(10.4373333644067,1.33274828542264,2.93611699239956));
#24455=CARTESIAN_POINT('Ctrl Pts',(10.4308865932805,1.42629874029213,2.88994627388488));
#24456=CARTESIAN_POINT('Ctrl Pts',(10.4244437526675,1.51979215865555,2.84380370506193));
#24457=CARTESIAN_POINT('Ctrl Pts',(10.4180009120544,1.61108457729918,2.79310051679673));
#24458=CARTESIAN_POINT('Ctrl Pts',(10.4115580714414,1.69973099746441,2.738070871756));
#24459=CARTESIAN_POINT('Ctrl Pts',(10.4051182487401,1.78833589447452,2.6830670033285));
#24460=CARTESIAN_POINT('Ctrl Pts',(10.3986784260388,1.87429694022193,2.62374091607416));
#24461=CARTESIAN_POINT('Ctrl Pts',(10.3922386033375,1.95719559860731,2.56037164319795));
#24462=CARTESIAN_POINT('Ctrl Pts',(10.385800888716,2.04006712006665,2.49702311429161));
#24463=CARTESIAN_POINT('Ctrl Pts',(10.3793631740946,2.11987795063644,2.42963426812137));
#24464=CARTESIAN_POINT('Ctrl Pts',(10.3729254594731,2.19624058877033,2.35852598856527));
#24465=CARTESIAN_POINT('Ctrl Pts',(10.3664879734686,2.27260051510442,2.28742023421551));
#24466=CARTESIAN_POINT('Ctrl Pts',(10.3600504874641,2.3455122115232,2.21259556466524));
#24467=CARTESIAN_POINT('Ctrl Pts',(10.3536130014596,2.4146232787165,2.13441139061344));
#24468=CARTESIAN_POINT('Ctrl Pts',(10.3471760507783,2.4837285988282,2.05623371813723));
#24469=CARTESIAN_POINT('Ctrl Pts',(10.340739100097,2.5490336708833,1.97469738502973));
#24470=CARTESIAN_POINT('Ctrl Pts',(10.3343021494157,2.61022524172581,1.89019621996168));
#24471=CARTESIAN_POINT('Ctrl Pts',(10.3278634462972,2.67143347175855,1.80567204974826));
#24472=CARTESIAN_POINT('Ctrl Pts',(10.3214247431787,2.72852574152598,1.71818174357321));
#24473=CARTESIAN_POINT('Ctrl Pts',(10.3149860400602,2.78123115456013,1.62814951015074));
#24474=CARTESIAN_POINT('Ctrl Pts',(10.3121359164215,2.80456146515386,1.58829629872004));
#24475=CARTESIAN_POINT('Ctrl Pts',(10.3092857927828,2.82703277931589,1.54794537985008));
#24476=CARTESIAN_POINT('Ctrl Pts',(10.3064356691441,2.84862442585766,1.50713517738361));
#24477=CARTESIAN_POINT('Ctrl Pts',(10.4912624831434,-2.84862442585767,1.50713517738359));
#24478=CARTESIAN_POINT('Ctrl Pts',(10.4848229789318,-2.7998407531234,1.59934081614728));
#24479=CARTESIAN_POINT('Ctrl Pts',(10.4783834747201,-2.74656357692504,1.68920009129343));
#24480=CARTESIAN_POINT('Ctrl Pts',(10.4719439705085,-2.68904405066309,1.7762769086191));
#24481=CARTESIAN_POINT('Ctrl Pts',(10.4655059569842,-2.63153783965492,1.86333356844357));
#24482=CARTESIAN_POINT('Ctrl Pts',(10.4590679434599,-2.56979144488121,1.94760873730506));
#24483=CARTESIAN_POINT('Ctrl Pts',(10.4526299299357,-2.50409982107675,2.02869456759351));
#24484=CARTESIAN_POINT('Ctrl Pts',(10.4461925020982,-2.43841417345056,2.10977302124322));
#24485=CARTESIAN_POINT('Ctrl Pts',(10.4397550742607,-2.36878425171169,2.18766242004355));
#24486=CARTESIAN_POINT('Ctrl Pts',(10.4333176464233,-2.29554560560487,2.26198760719155));
#24487=CARTESIAN_POINT('Ctrl Pts',(10.4268798998167,-2.2223033328601,2.33631647478094));
#24488=CARTESIAN_POINT('Ctrl Pts',(10.4204421532101,-2.14545224721117,2.40708050962087));
#24489=CARTESIAN_POINT('Ctrl Pts',(10.4140044066035,-2.06536483265434,2.47394132317942));
#24490=CARTESIAN_POINT('Ctrl Pts',(10.4075632723932,-1.98523527533568,2.54083731953612));
#24491=CARTESIAN_POINT('Ctrl Pts',(10.4011221381828,-1.90186627796118,2.60382574688035));
#24492=CARTESIAN_POINT('Ctrl Pts',(10.3946810039725,-1.81566359955142,2.66260835568508));
#24493=CARTESIAN_POINT('Ctrl Pts',(10.3882383279055,-1.72944028623876,2.72140503567004));
#24494=CARTESIAN_POINT('Ctrl Pts',(10.3817956518385,-1.64038225773539,2.77599368227329));
#24495=CARTESIAN_POINT('Ctrl Pts',(10.3753529757714,-1.54892361204772,2.82611981461173));
#24496=CARTESIAN_POINT('Ctrl Pts',(10.3689054690181,-1.4573963911248,2.87628353127358));
#24497=CARTESIAN_POINT('Ctrl Pts',(10.3624579622648,-1.36346529368264,2.92197787261881));
#24498=CARTESIAN_POINT('Ctrl Pts',(10.3560104555115,-1.26758849229933,2.96299459612911));
#24499=CARTESIAN_POINT('Ctrl Pts',(10.3531640522171,-1.22526142638758,2.98110239211788));
#24500=CARTESIAN_POINT('Ctrl Pts',(10.3503176489226,-1.18255541593426,2.99829915258518));
#24501=CARTESIAN_POINT('Ctrl Pts',(10.3474712456282,-1.13951104417291,3.01456997641587));
#24502=CARTESIAN_POINT('Ctrl Pts',(10.3411636821617,-1.04412571796369,3.05062574341341));
#24503=CARTESIAN_POINT('Ctrl Pts',(10.3348561186953,-0.946950142990533,
3.08217952913117));
#24504=CARTESIAN_POINT('Ctrl Pts',(10.3285485552288,-0.848436505241506,
3.10906305164009));
#24505=CARTESIAN_POINT('Ctrl Pts',(10.3222451395699,-0.749987649340766,
3.13592889574106));
#24506=CARTESIAN_POINT('Ctrl Pts',(10.3159417239111,-0.650202874771774,
3.15813048003906));
#24507=CARTESIAN_POINT('Ctrl Pts',(10.3096383082522,-0.54955031933025,3.17554908779947));
#24508=CARTESIAN_POINT('Ctrl Pts',(10.3033376504346,-0.448941800929435,
3.19296007465114));
#24509=CARTESIAN_POINT('Ctrl Pts',(10.2970369926171,-0.347466659599731,
3.20559218039583));
#24510=CARTESIAN_POINT('Ctrl Pts',(10.2907363347995,-0.245603373769911,
3.21337774705882));
#24511=CARTESIAN_POINT('Ctrl Pts',(10.2844370476819,-0.143762248165569,
3.2211616199819));
#24512=CARTESIAN_POINT('Ctrl Pts',(10.2781377605642,-0.0415335536093207,
3.22410102267434));
#24513=CARTESIAN_POINT('Ctrl Pts',(10.2718384734466,0.0605996360431658,
3.22218020082854));
#24514=CARTESIAN_POINT('Ctrl Pts',(10.2655370634233,0.162767245323142,3.22025873165181));
#24515=CARTESIAN_POINT('Ctrl Pts',(10.2592356534001,0.264838876269155,3.21347376886252));
#24516=CARTESIAN_POINT('Ctrl Pts',(10.2529342433769,0.366332180125763,3.20186169225098));
#24517=CARTESIAN_POINT('Ctrl Pts',(10.2466318509943,0.467841306299447,3.19024780537265));
#24518=CARTESIAN_POINT('Ctrl Pts',(10.2403294586116,0.568771520358791,3.17380536012273));
#24519=CARTESIAN_POINT('Ctrl Pts',(10.2340270662289,0.668647573229539,3.15262239814955));
#24520=CARTESIAN_POINT('Ctrl Pts',(10.227719370176,0.768607675080177,3.13142161001792));
#24521=CARTESIAN_POINT('Ctrl Pts',(10.2214116741231,0.867511444986111,3.1054724289363));
#24522=CARTESIAN_POINT('Ctrl Pts',(10.2151039780701,0.96489578616085,3.07491360599758));
#24523=CARTESIAN_POINT('Ctrl Pts',(10.2112959880844,1.02368723597793,3.05646508045848));
#24524=CARTESIAN_POINT('Ctrl Pts',(10.2074879980988,1.08192519998495,3.0363374941559));
#24525=CARTESIAN_POINT('Ctrl Pts',(10.2036800081131,1.13951104417291,3.01456997641587));
#24526=CARTESIAN_POINT('Ctrl Pts',(10.197232755895,1.23700879575944,2.97771571010789));
#24527=CARTESIAN_POINT('Ctrl Pts',(10.1907855036769,1.33276939769849,2.93610767816709));
#24528=CARTESIAN_POINT('Ctrl Pts',(10.1843382514589,1.42632620359115,2.88993271953678));
#24529=CARTESIAN_POINT('Ctrl Pts',(10.1778949245562,1.51982604878806,2.84378587385608));
#24530=CARTESIAN_POINT('Ctrl Pts',(10.1714515976536,1.61112443098708,2.79307780825953));
#24531=CARTESIAN_POINT('Ctrl Pts',(10.165008270751,1.69977630378595,2.73804274612135));
#24532=CARTESIAN_POINT('Ctrl Pts',(10.1585679586868,1.78838669629298,2.68303343493877));
#24533=CARTESIAN_POINT('Ctrl Pts',(10.1521276466227,1.87435272449252,2.62370136121625));
#24534=CARTESIAN_POINT('Ctrl Pts',(10.1456873345586,1.95725580776304,2.56032561708034));
#24535=CARTESIAN_POINT('Ctrl Pts',(10.1392491296191,2.04013176701713,2.49697060805654));
#24536=CARTESIAN_POINT('Ctrl Pts',(10.1328109246796,2.11994647721657,2.42957479584968));
#24537=CARTESIAN_POINT('Ctrl Pts',(10.1263727197401,2.1963123943059,2.35845912178233));
#24538=CARTESIAN_POINT('Ctrl Pts',(10.1199347470207,2.27267555694775,2.28734601279109));
#24539=CARTESIAN_POINT('Ctrl Pts',(10.1134967743013,2.34558989296914,2.21251356423462));
#24540=CARTESIAN_POINT('Ctrl Pts',(10.1070588015818,2.41470296197287,2.1343212429106));
#24541=CARTESIAN_POINT('Ctrl Pts',(10.1006213673406,2.48381025029353,2.05613546166699));
#24542=CARTESIAN_POINT('Ctrl Pts',(10.0941839330994,2.5491166566131,1.97459065475291));
#24543=CARTESIAN_POINT('Ctrl Pts',(10.0877464988581,2.61030888683252,1.89008070669567));
#24544=CARTESIAN_POINT('Ctrl Pts',(10.0813073214399,2.67151768714493,1.80554787439817));
#24545=CARTESIAN_POINT('Ctrl Pts',(10.0748681440218,2.72860986399238,1.71804860534506));
#24546=CARTESIAN_POINT('Ctrl Pts',(10.0684289666036,2.781314479966,1.62800716399882));
#24547=CARTESIAN_POINT('Ctrl Pts',(10.0655822346017,2.80461495876892,1.58820023899394));
#24548=CARTESIAN_POINT('Ctrl Pts',(10.0627355025998,2.82705847329692,1.54789681585724));
#24549=CARTESIAN_POINT('Ctrl Pts',(10.0598887705979,2.84862442585767,1.50713517738359));
#24550=CARTESIAN_POINT('Origin',(13.3346225254169,0.,0.));
#24551=CARTESIAN_POINT('',(11.0238490761438,1.87105265221536,-2.62398161867378));
#24552=CARTESIAN_POINT('Ctrl Pts',(11.0238490761438,1.87105265221536,-2.62398161867378));
#24553=CARTESIAN_POINT('Ctrl Pts',(11.0171010612196,1.78198399703447,-2.68749278899581));
#24554=CARTESIAN_POINT('Ctrl Pts',(11.0103530462954,1.6897328614071,-2.74642706210009));
#24555=CARTESIAN_POINT('Ctrl Pts',(11.0036050313713,1.59477453685249,-2.80050205125919));
#24556=CARTESIAN_POINT('Ctrl Pts',(10.9968363324979,1.49952514697184,-2.85474279054524));
#24557=CARTESIAN_POINT('Ctrl Pts',(10.9900676336245,1.40155221258743,-2.90409427015761));
#24558=CARTESIAN_POINT('Ctrl Pts',(10.9832989347511,1.30135856293772,-2.94831875026576));
#24559=CARTESIAN_POINT('Ctrl Pts',(10.9765302358777,1.20116491328801,-2.99254323037392));
#24560=CARTESIAN_POINT('Ctrl Pts',(10.9697615370043,1.09875083290288,-3.03164061448522));
#24561=CARTESIAN_POINT('Ctrl Pts',(10.962992838131,0.99463811646416,-3.06542208835531));
#24562=CARTESIAN_POINT('Ctrl Pts',(10.9566676158604,0.897346733735724,-3.09699024271578));
#24563=CARTESIAN_POINT('Ctrl Pts',(10.9503423935899,0.798480009417802,-3.12394554759593));
#24564=CARTESIAN_POINT('Ctrl Pts',(10.9440171713194,0.698500851313238,-3.14614273726013));
#24565=CARTESIAN_POINT('Ctrl Pts',(10.9376957912064,0.598582423987644,-3.16832644358796));
#24566=CARTESIAN_POINT('Ctrl Pts',(10.9313744110934,0.497553302409718,-3.18575769915854));
#24567=CARTESIAN_POINT('Ctrl Pts',(10.9250530309804,0.395889691787329,-3.19834158814166));
#24568=CARTESIAN_POINT('Ctrl Pts',(10.9187341516616,0.294266300193852,-3.21092049882634));
#24569=CARTESIAN_POINT('Ctrl Pts',(10.9124152723428,0.192009320978601,-3.21865581095524));
#24570=CARTESIAN_POINT('Ctrl Pts',(10.906096393024,0.0896026158676177,-3.22150414150435));
#24571=CARTESIAN_POINT('Ctrl Pts',(10.8997786757475,-0.0127852566451852,
-3.22435194824533));
#24572=CARTESIAN_POINT('Ctrl Pts',(10.8934609584709,-0.115322395341751,
-3.22231455286083));
#24573=CARTESIAN_POINT('Ctrl Pts',(10.8871432411943,-0.217523020598734,
-3.21540064346725));
#24574=CARTESIAN_POINT('Ctrl Pts',(10.8808234830682,-0.319756660328726,
-3.20848450063259));
#24575=CARTESIAN_POINT('Ctrl Pts',(10.874503724942,-0.421653164719666,-3.19668872134875));
#24576=CARTESIAN_POINT('Ctrl Pts',(10.8681839668158,-0.522730172436479,
-3.18007401318342));
#24577=CARTESIAN_POINT('Ctrl Pts',(10.8618631165486,-0.623824647649185,
-3.16345643376822));
#24578=CARTESIAN_POINT('Ctrl Pts',(10.8555422662814,-0.724098945437443,
-3.14201834014415));
#24579=CARTESIAN_POINT('Ctrl Pts',(10.8492214160142,-0.823080366901728,
-3.11587167131782));
#24580=CARTESIAN_POINT('Ctrl Pts',(10.8428959208975,-0.922134524435214,
-3.08970578872506));
#24581=CARTESIAN_POINT('Ctrl Pts',(10.8365704257808,-1.01989351873125,-3.05882453322215));
#24582=CARTESIAN_POINT('Ctrl Pts',(10.8302449306641,-1.11589942283804,-3.0233898261074));
#24583=CARTESIAN_POINT('Ctrl Pts',(10.8281435552309,-1.14779328167668,-3.0116181589665));
#24584=CARTESIAN_POINT('Ctrl Pts',(10.8260421797977,-1.17949382102355,-2.99934436333468));
#24585=CARTESIAN_POINT('Ctrl Pts',(10.8239408043644,-1.21098474892435,-2.98657554740754));
#24586=CARTESIAN_POINT('Ctrl Pts',(10.8174850956538,-1.30772912612473,-2.94734802294879));
#24587=CARTESIAN_POINT('Ctrl Pts',(10.8110293869433,-1.4026126142313,-2.90339672979654));
#24588=CARTESIAN_POINT('Ctrl Pts',(10.8045736782327,-1.49517238600333,-2.85492155735199));
#24589=CARTESIAN_POINT('Ctrl Pts',(10.7981215694289,-1.58768054352744,-2.80647341619242));
#24590=CARTESIAN_POINT('Ctrl Pts',(10.7916694606252,-1.67786723238977,-2.75350659665608));
#24591=CARTESIAN_POINT('Ctrl Pts',(10.7852173518214,-1.76529252213514,-2.69626776745073));
#24592=CARTESIAN_POINT('Ctrl Pts',(10.7787679761062,-1.8526807788622,-2.63905318439448));
#24593=CARTESIAN_POINT('Ctrl Pts',(10.772318600391,-1.93730965183885,-2.57757040437331));
#24594=CARTESIAN_POINT('Ctrl Pts',(10.7658692246759,-2.01876688252812,-2.5121102357396));
#24595=CARTESIAN_POINT('Ctrl Pts',(10.7591208535027,-2.10400050074261,-2.44361530933014));
#24596=CARTESIAN_POINT('Ctrl Pts',(10.7523724823295,-2.18576095349918,-2.37076556946754));
#24597=CARTESIAN_POINT('Ctrl Pts',(10.7456241111564,-2.26361331126617,-2.29394253187794));
#24598=CARTESIAN_POINT('Ctrl Pts',(10.7391767794815,-2.33799273695526,-2.22054650920761));
#24599=CARTESIAN_POINT('Ctrl Pts',(10.7327294478066,-2.40880496089534,-2.14352435156969));
#24600=CARTESIAN_POINT('Ctrl Pts',(10.7262821161317,-2.47570777028153,-2.06324710072925));
#24601=CARTESIAN_POINT('Ctrl Pts',(10.7198351359104,-2.54260693269592,-1.98297422592133));
#24602=CARTESIAN_POINT('Ctrl Pts',(10.7133881556892,-2.6055968665912,-1.89944690412764));
#24603=CARTESIAN_POINT('Ctrl Pts',(10.7069411754679,-2.66437553899544,-1.8130693725566));
#24604=CARTESIAN_POINT('Ctrl Pts',(10.7004927241863,-2.72316762341218,-1.72667213151467));
#24605=CARTESIAN_POINT('Ctrl Pts',(10.6940442729046,-2.77774631691511,-1.63742369544976));
#24606=CARTESIAN_POINT('Ctrl Pts',(10.6875958216229,-2.82785288593765,-1.54575729595371));
#24607=CARTESIAN_POINT('Ctrl Pts',(10.6866934712812,-2.83486444231021,-1.53293015292487));
#24608=CARTESIAN_POINT('Ctrl Pts',(10.6857911209396,-2.84178850148947,-1.52005570463342));
#24609=CARTESIAN_POINT('Ctrl Pts',(10.6848887705979,-2.84862442585766,-1.5071351773836));
#24610=CARTESIAN_POINT('',(11.0238490761438,-1.87158653173898,-2.62360084935061));
#24611=CARTESIAN_POINT('Origin',(11.0238490761438,0.,0.));
#24612=CARTESIAN_POINT('Ctrl Pts',(11.0238490761438,-1.87158653173898,-2.62360084935061));
#24613=CARTESIAN_POINT('Ctrl Pts',(11.0084294243278,-2.07493559933386,-2.47853862456651));
#24614=CARTESIAN_POINT('Ctrl Pts',(10.9932849210064,-2.26073288354223,-2.31032499875892));
#24615=CARTESIAN_POINT('Ctrl Pts',(10.9624483041142,-2.58973185199326,-1.93437311771314));
#24616=CARTESIAN_POINT('Ctrl Pts',(10.9468547252081,-2.73181447276606,-1.72791675726662));
#24617=CARTESIAN_POINT('Ctrl Pts',(10.9314356691441,-2.84862442585767,-1.5071351773836));
#24618=CARTESIAN_POINT('Ctrl Pts',(11.1008112312664,1.68942544263115,3.40346056344526));
#24619=CARTESIAN_POINT('Ctrl Pts',(11.0751571795589,2.12830620414844,3.18560690803575));
#24620=CARTESIAN_POINT('Ctrl Pts',(11.0495031278513,2.52436782889846,2.88189967479167));
#24621=CARTESIAN_POINT('Ctrl Pts',(11.0238490761438,2.84862442585767,2.51456577037539));
#24622=CARTESIAN_POINT('Ctrl Pts',(11.0751571795589,1.70918178686444,3.44326104044715));
#24623=CARTESIAN_POINT('Ctrl Pts',(11.0495031278513,2.15319487277031,3.22285977820035));
#24624=CARTESIAN_POINT('Ctrl Pts',(11.0238490761438,2.55388808977572,2.91560095605822));
#24625=CARTESIAN_POINT('Ctrl Pts',(10.9981950244362,2.88193658236276,2.54397140480186));
#24626=CARTESIAN_POINT('Ctrl Pts',(11.0495031278513,1.72893813109773,3.48306151744904));
#24627=CARTESIAN_POINT('Ctrl Pts',(11.0238490761438,2.17808354139218,3.26011264836494));
#24628=CARTESIAN_POINT('Ctrl Pts',(10.9981950244362,2.58340835065299,2.94930223732478));
#24629=CARTESIAN_POINT('Ctrl Pts',(10.9725409727286,2.91524873886784,2.57337703922832));
#24630=CARTESIAN_POINT('Ctrl Pts',(11.0238490761438,1.74869447533101,3.52286199445093));
#24631=CARTESIAN_POINT('Ctrl Pts',(10.9981950244362,2.20297221001404,3.29736551852953));
#24632=CARTESIAN_POINT('Ctrl Pts',(10.9725409727286,2.61292861153025,2.98300351859134));
#24633=CARTESIAN_POINT('Ctrl Pts',(10.9468869210211,2.94856089537293,2.60278267365479));
#24634=CARTESIAN_POINT('',(11.0238490761438,1.74869447533103,3.52286199445092));
#24635=CARTESIAN_POINT('Ctrl Pts',(11.0238490761438,1.74869447533103,3.52286199445092));
#24636=CARTESIAN_POINT('Ctrl Pts',(11.0006887763626,2.15881326042978,3.31928534147352));
#24637=CARTESIAN_POINT('Ctrl Pts',(10.9775284765815,2.53280859423868,3.0432801490367));
#24638=CARTESIAN_POINT('Ctrl Pts',(10.9543681768003,2.84860418144656,2.71177492056083));
#24639=CARTESIAN_POINT('Origin',(11.0238490761448,0.32028972767158,0.987026521741422));
#24640=CARTESIAN_POINT('Ctrl Pts',(3.61717341366717,2.84754707936762,-1.50592664679481));
#24641=CARTESIAN_POINT('Ctrl Pts',(3.56923138188706,2.48464894021009,-2.1921402390435));
#24642=CARTESIAN_POINT('Ctrl Pts',(3.47335893760189,1.24438661619661,-3.28829531364372));
#24643=CARTESIAN_POINT('Ctrl Pts',(3.32954446153663,-1.24438661619659,-3.28829531364374));
#24644=CARTESIAN_POINT('Ctrl Pts',(3.23367201725147,-2.48464894021008,-2.19214023904351));
#24645=CARTESIAN_POINT('Ctrl Pts',(3.18572998547137,-2.84754707936761,-1.50592664679483));
#24646=CARTESIAN_POINT('Ctrl Pts',(3.48019371320366,3.05727954735629,-1.61684376368135));
#24647=CARTESIAN_POINT('Ctrl Pts',(3.43225168142354,2.66765260609905,-2.35359954759826));
#24648=CARTESIAN_POINT('Ctrl Pts',(3.33637923713838,1.33604033389561,-3.53049053373441));
#24649=CARTESIAN_POINT('Ctrl Pts',(3.19256476107312,-1.33604033389558,-3.53049053373443));
#24650=CARTESIAN_POINT('Ctrl Pts',(3.09669231678796,-2.66765260609903,-2.35359954759828));
#24651=CARTESIAN_POINT('Ctrl Pts',(3.04875028500786,-3.05727954735627,-1.61684376368138));
#24652=CARTESIAN_POINT('Ctrl Pts',(3.34321401274013,3.26701201534495,-1.7277608805679));
#24653=CARTESIAN_POINT('Ctrl Pts',(3.29527198096003,2.85065627198801,-2.51505885615301));
#24654=CARTESIAN_POINT('Ctrl Pts',(3.19939953667487,1.42769405159462,-3.77268575382511));
#24655=CARTESIAN_POINT('Ctrl Pts',(3.05558506060961,-1.42769405159458,-3.77268575382512));
#24656=CARTESIAN_POINT('Ctrl Pts',(2.95971261632444,-2.85065627198798,-2.51505885615305));
#24657=CARTESIAN_POINT('Ctrl Pts',(2.91177058454434,-3.26701201534493,-1.72776088056793));
#24658=CARTESIAN_POINT('Ctrl Pts',(3.20623431227662,3.47674448333362,-1.83867799745444));
#24659=CARTESIAN_POINT('Ctrl Pts',(3.15829228049652,3.03365993787697,-2.67651816470778));
#24660=CARTESIAN_POINT('Ctrl Pts',(3.06241983621135,1.51934776929363,-4.01488097391579));
#24661=CARTESIAN_POINT('Ctrl Pts',(2.91860536014609,-1.51934776929357,-4.01488097391582));
#24662=CARTESIAN_POINT('Ctrl Pts',(2.82273291586093,-3.03365993787694,-2.67651816470782));
#24663=CARTESIAN_POINT('Ctrl Pts',(2.77479088408083,-3.47674448333358,-1.83867799745449));
#24664=CARTESIAN_POINT('',(3.02384907614375,0.656739510617909,-3.87731438084271));
#24665=CARTESIAN_POINT('Ctrl Pts',(3.02384907614375,0.656739510617945,-3.8773143808427));
#24666=CARTESIAN_POINT('Ctrl Pts',(3.02384907614375,0.535250361035218,-3.88669383362465));
#24667=CARTESIAN_POINT('Ctrl Pts',(3.02384907614375,0.413571785996884,-3.89044850980247));
#24668=CARTESIAN_POINT('Ctrl Pts',(3.02384907614375,0.292110716985867,-3.88864428500737));
#24669=CARTESIAN_POINT('Ctrl Pts',(3.02384907614375,0.170355994992987,-3.88683569818915));
#24670=CARTESIAN_POINT('Ctrl Pts',(3.02384907614375,0.0488189541319484,
-3.87944114112614));
#24671=CARTESIAN_POINT('Ctrl Pts',(3.02384907614375,-0.0720841979465033,
-3.86647526033853));
#24672=CARTESIAN_POINT('Ctrl Pts',(3.02384907614375,-0.190730889393864,
-3.8537513666211));
#24673=CARTESIAN_POINT('Ctrl Pts',(3.02384907614375,-0.308767877441656,
-3.83566186693603));
#24674=CARTESIAN_POINT('Ctrl Pts',(3.02384907614376,-0.425783805981553,
-3.81217453448968));
#24675=CARTESIAN_POINT('Ctrl Pts',(3.02384907614376,-0.503663330587906,
-3.79654262601349));
#24676=CARTESIAN_POINT('Ctrl Pts',(3.02384907614375,-0.581090188608406,
-3.77851880307661));
#24677=CARTESIAN_POINT('Ctrl Pts',(3.02384907614375,-0.657936144092792,
-3.7580828506885));
#24678=CARTESIAN_POINT('Ctrl Pts',(3.02384907614375,-0.701243993644106,
-3.7465658209908));
#24679=CARTESIAN_POINT('Ctrl Pts',(3.02384907614375,-0.744367230915085,
-3.73428252775564));
#24680=CARTESIAN_POINT('Ctrl Pts',(3.02384907614375,-0.787281908431366,
-3.72122819379682));
#24681=CARTESIAN_POINT('Ctrl Pts',(3.02384907614375,-0.813120406729992,
-3.71336830982923));
#24682=CARTESIAN_POINT('Ctrl Pts',(3.02384907614375,-0.838889973343018,
-3.70522654477816));
#24683=CARTESIAN_POINT('Ctrl Pts',(3.02384907614375,-0.864545043675188,
-3.69681537290214));
#24684=CARTESIAN_POINT('Ctrl Pts',(3.02384907614375,-0.976135859364577,
-3.66022964078777));
#24685=CARTESIAN_POINT('Ctrl Pts',(3.02384907614374,-1.08569188131441,-3.6185141205333));
#24686=CARTESIAN_POINT('Ctrl Pts',(3.02384907614375,-1.19283428496982,-3.57167684930927));
#24687=CARTESIAN_POINT('Ctrl Pts',(3.02384907614375,-1.23792927339732,-3.55196358796956));
#24688=CARTESIAN_POINT('Ctrl Pts',(3.02384907614375,-1.28259643581524,-3.53134245497185));
#24689=CARTESIAN_POINT('Ctrl Pts',(3.02384907614375,-1.32680617741714,-3.50981161930699));
#24690=CARTESIAN_POINT('Ctrl Pts',(3.02384907614375,-1.43295276301009,-3.45811657183608));
#24691=CARTESIAN_POINT('Ctrl Pts',(3.02384907614375,-1.53646498001698,-3.40117991937055));
#24692=CARTESIAN_POINT('Ctrl Pts',(3.02384907614376,-1.63705571648453,-3.33929701181508));
#24693=CARTESIAN_POINT('Ctrl Pts',(3.02384907614375,-1.73742382560611,-3.27755106346635));
#24694=CARTESIAN_POINT('Ctrl Pts',(3.02384907614375,-1.8348839104347,-3.21088000755977));
#24695=CARTESIAN_POINT('Ctrl Pts',(3.02384907614375,-1.92911029541134,-3.13954526120031));
#24696=CARTESIAN_POINT('Ctrl Pts',(3.02384907614375,-1.98067917691666,-3.10050467736453));
#24697=CARTESIAN_POINT('Ctrl Pts',(3.02384907614375,-2.0312787351562,-3.06006671454503));
#24698=CARTESIAN_POINT('Ctrl Pts',(3.02384907614375,-2.08084955088305,-3.01827133086486));
#24699=CARTESIAN_POINT('Ctrl Pts',(3.02384907614375,-2.10068222578663,-3.00154951088178));
#24700=CARTESIAN_POINT('Ctrl Pts',(3.02384907614375,-2.12033510199988,-2.98462300334752));
#24701=CARTESIAN_POINT('Ctrl Pts',(3.02384907614375,-2.13979707289644,-2.96750248510469));
#24702=CARTESIAN_POINT('Ctrl Pts',(3.02384907614375,-2.22654408713123,-2.89119192809017));
#24703=CARTESIAN_POINT('Ctrl Pts',(3.02384907614375,-2.30955532853918,-2.81098435880976));
#24704=CARTESIAN_POINT('Ctrl Pts',(3.02384907614375,-2.38857390968403,-2.7271714464646));
#24705=CARTESIAN_POINT('Ctrl Pts',(3.02384907614375,-2.46731588582698,-2.64365192170554));
#24706=CARTESIAN_POINT('Ctrl Pts',(3.02384907614375,-2.54209358615361,-2.55655152694044));
#24707=CARTESIAN_POINT('Ctrl Pts',(3.02384907614375,-2.61261003092816,-2.46613020119734));
#24708=CARTESIAN_POINT('Ctrl Pts',(3.02384907614375,-2.68187774753533,-2.37731008573575));
#24709=CARTESIAN_POINT('Ctrl Pts',(3.02384907614376,-2.74703411602985,-2.28528492198977));
#24710=CARTESIAN_POINT('Ctrl Pts',(3.02384907614376,-2.80775053351277,-2.19028389748536));
#24711=CARTESIAN_POINT('Ctrl Pts',(3.02384907614376,-2.82131446704313,-2.16906084719494));
#24712=CARTESIAN_POINT('Ctrl Pts',(3.02384907614375,-2.83465661709219,-2.14768923548602));
#24713=CARTESIAN_POINT('Ctrl Pts',(3.02384907614375,-2.84777296580223,-2.12617155036607));
#24714=CARTESIAN_POINT('Ctrl Pts',(3.15165719587644,2.84680317627431,-2.71057532546662));
#24715=CARTESIAN_POINT('Ctrl Pts',(3.12190753622973,2.44054601589642,-3.13625204053632));
#24716=CARTESIAN_POINT('Ctrl Pts',(3.07930482965216,1.72451086510843,-3.61812557132028));
#24717=CARTESIAN_POINT('Ctrl Pts',(3.03670212307461,0.907492295035082,-3.83572132698351));
#24718=CARTESIAN_POINT('Ctrl Pts',(3.02384907614375,0.656739510617909,-3.87731438084271));
#24719=CARTESIAN_POINT('Ctrl Pts',(4.86717770674282,2.84754200119055,-1.50592095217182));
#24720=CARTESIAN_POINT('Ctrl Pts',(4.81923562020286,2.48464485522122,-2.19213412441211));
#24721=CARTESIAN_POINT('Ctrl Pts',(4.72336312115783,1.24432634307189,-3.28827073269437));
#24722=CARTESIAN_POINT('Ctrl Pts',(4.57954853557285,-1.24432634307187,-3.28827073269438));
#24723=CARTESIAN_POINT('Ctrl Pts',(4.48367603652783,-2.48464485522121,-2.19213412441212));
#24724=CARTESIAN_POINT('Ctrl Pts',(4.43573394998787,-2.84754200119054,-1.50592095217184));
#24725=CARTESIAN_POINT('Ctrl Pts',(4.73019663001395,3.05727666799789,-1.61683901027592));
#24726=CARTESIAN_POINT('Ctrl Pts',(4.68225454347398,2.66765046519168,-2.35359496326481));
#24727=CARTESIAN_POINT('Ctrl Pts',(4.58638204442896,1.33597674571904,-3.5304671133643));
#24728=CARTESIAN_POINT('Ctrl Pts',(4.44256745884398,-1.33597674571901,-3.53046711336431));
#24729=CARTESIAN_POINT('Ctrl Pts',(4.34669495979896,-2.66765046519166,-2.35359496326483));
#24730=CARTESIAN_POINT('Ctrl Pts',(4.29875287325899,-3.05727666799787,-1.61683901027595));
#24731=CARTESIAN_POINT('Ctrl Pts',(4.59321555328507,3.26701133480523,-1.72775706838004));
#24732=CARTESIAN_POINT('Ctrl Pts',(4.54527346674511,2.85065607516215,-2.51505580211753));
#24733=CARTESIAN_POINT('Ctrl Pts',(4.44940096770009,1.4276271483662,-3.77266349403423));
#24734=CARTESIAN_POINT('Ctrl Pts',(4.30558638211511,-1.42762714836615,-3.77266349403425));
#24735=CARTESIAN_POINT('Ctrl Pts',(4.20971388307008,-2.85065607516212,-2.51505580211756));
#24736=CARTESIAN_POINT('Ctrl Pts',(4.16177179653012,-3.26701133480521,-1.72775706838007));
#24737=CARTESIAN_POINT('Ctrl Pts',(4.4562344765562,3.47674600161257,-1.83867512648414));
#24738=CARTESIAN_POINT('Ctrl Pts',(4.40829239001624,3.03366168513261,-2.67651664097024));
#24739=CARTESIAN_POINT('Ctrl Pts',(4.31241989097121,1.51927755101335,-4.01485987470417));
#24740=CARTESIAN_POINT('Ctrl Pts',(4.16860530538623,-1.5192775510133,-4.01485987470418));
#24741=CARTESIAN_POINT('Ctrl Pts',(4.07273280634121,-3.03366168513258,-2.67651664097028));
#24742=CARTESIAN_POINT('Ctrl Pts',(4.02479071980125,-3.47674600161254,-1.83867512648419));
#24743=CARTESIAN_POINT('Ctrl Pts',(4.40165719587644,2.84679199383306,-2.71057163545836));
#24744=CARTESIAN_POINT('Ctrl Pts',(4.37190753622973,2.44052493609236,-3.13624479621667));
#24745=CARTESIAN_POINT('Ctrl Pts',(4.29422746407797,1.13490282761621,-4.01485987470402));
#24746=CARTESIAN_POINT('Ctrl Pts',(4.18679773227948,-1.13490282761596,-4.01485987470424));
#24747=CARTESIAN_POINT('Ctrl Pts',(4.10911766012771,-2.44052493609232,-3.1362447962167));
#24748=CARTESIAN_POINT('Ctrl Pts',(4.079368000481,-2.84679199383302,-2.7105716354584));
#24749=CARTESIAN_POINT('Ctrl Pts',(6.11718155610245,2.8475374478682,-1.50591584613134));
#24750=CARTESIAN_POINT('Ctrl Pts',(6.06923942046241,2.484641192321,-2.19212864202859));
#24751=CARTESIAN_POINT('Ctrl Pts',(5.9733668723173,1.24427323296847,-3.28824777229012));
#24752=CARTESIAN_POINT('Ctrl Pts',(5.82955218853213,-1.24427323296843,-3.28824777229013));
#24753=CARTESIAN_POINT('Ctrl Pts',(5.73367964038703,-2.48464119232097,-2.19212864202862));
#24754=CARTESIAN_POINT('Ctrl Pts',(5.68573750474698,-2.84753744786818,-1.50591584613138));
#24755=CARTESIAN_POINT('Ctrl Pts',(5.98019924535379,3.05727408623409,-1.61683474816929));
#24756=CARTESIAN_POINT('Ctrl Pts',(5.93225710971374,2.66764854543341,-2.35359085303088));
#24757=CARTESIAN_POINT('Ctrl Pts',(5.83638456156864,1.33592073185802,-3.53044512579308));
#24758=CARTESIAN_POINT('Ctrl Pts',(5.69256987778346,-1.33592073185797,-3.5304451257931));
#24759=CARTESIAN_POINT('Ctrl Pts',(5.59669732963837,-2.66764854543338,-2.35359085303092));
#24760=CARTESIAN_POINT('Ctrl Pts',(5.54875519399832,-3.05727408623406,-1.61683474816934));
#24761=CARTESIAN_POINT('Ctrl Pts',(5.84321693460512,3.26701072459998,-1.72775365020725));
#24762=CARTESIAN_POINT('Ctrl Pts',(5.79527479896508,2.85065589854583,-2.51505306403319));
#24763=CARTESIAN_POINT('Ctrl Pts',(5.69940225081997,1.42756823074758,-3.77264247929604));
#24764=CARTESIAN_POINT('Ctrl Pts',(5.5555875670348,-1.42756823074751,-3.77264247929606));
#24765=CARTESIAN_POINT('Ctrl Pts',(5.4597150188897,-2.85065589854579,-2.51505306403324));
#24766=CARTESIAN_POINT('Ctrl Pts',(5.41177288324965,-3.26701072459995,-1.7277536502073));
#24767=CARTESIAN_POINT('Ctrl Pts',(5.70623462385646,3.47674736296587,-1.8386725522452));
#24768=CARTESIAN_POINT('Ctrl Pts',(5.65829248821641,3.03366325165824,-2.67651527503548));
#24769=CARTESIAN_POINT('Ctrl Pts',(5.56241994007131,1.51921572963714,-4.01483983279899));
#24770=CARTESIAN_POINT('Ctrl Pts',(5.41860525628614,-1.51921572963706,-4.01483983279902));
#24771=CARTESIAN_POINT('Ctrl Pts',(5.32273270814104,-3.03366325165819,-2.67651527503554));
#24772=CARTESIAN_POINT('Ctrl Pts',(5.27479057250099,-3.47674736296583,-1.83867255224527));
#24773=CARTESIAN_POINT('Ctrl Pts',(5.65165719587644,2.8467821456932,-2.71056813036079));
#24774=CARTESIAN_POINT('Ctrl Pts',(5.62190753622973,2.44050637155411,-3.13623791491845));
#24775=CARTESIAN_POINT('Ctrl Pts',(5.54422746407797,1.13485587203874,-4.01483983279886));
#24776=CARTESIAN_POINT('Ctrl Pts',(5.43679773227948,-1.13485587203849,-4.01483983279907));
#24777=CARTESIAN_POINT('Ctrl Pts',(5.35911766012771,-2.44050637155405,-3.1362379149185));
#24778=CARTESIAN_POINT('Ctrl Pts',(5.329368000481,-2.84678214569315,-2.71056813036084));
#24779=CARTESIAN_POINT('Ctrl Pts',(7.36718503194766,2.8475333363626,-1.505911235551));
#24780=CARTESIAN_POINT('Ctrl Pts',(7.31924285197185,2.48463788473179,-2.19212369184276));
#24781=CARTESIAN_POINT('Ctrl Pts',(7.22337025949097,1.24422607800448,-3.28822624954172));
#24782=CARTESIAN_POINT('Ctrl Pts',(7.07955548703428,-1.24422607800445,-3.28822624954172));
#24783=CARTESIAN_POINT('Ctrl Pts',(6.98368289455341,-2.48463788473177,-2.19212369184278));
#24784=CARTESIAN_POINT('Ctrl Pts',(6.9357407145776,-2.8475333363626,-1.50591123555103));
#24785=CARTESIAN_POINT('Ctrl Pts',(7.2302016069197,3.05727175498223,-1.61683089963102));
#24786=CARTESIAN_POINT('Ctrl Pts',(7.18225942694387,2.6676468118377,-2.35358714186614));
#24787=CARTESIAN_POINT('Ctrl Pts',(7.086386834463,1.33587101387704,-3.53042442325068));
#24788=CARTESIAN_POINT('Ctrl Pts',(6.94257206200631,-1.335871013877,-3.53042442325069));
#24789=CARTESIAN_POINT('Ctrl Pts',(6.84669946952544,-2.66764681183767,-2.35358714186617));
#24790=CARTESIAN_POINT('Ctrl Pts',(6.79875728954964,-3.05727175498221,-1.61683089963105));
#24791=CARTESIAN_POINT('Ctrl Pts',(7.09321818189172,3.26701017360185,-1.72775056371102));
#24792=CARTESIAN_POINT('Ctrl Pts',(7.04527600191591,2.85065573894362,-2.51505059188952));
#24793=CARTESIAN_POINT('Ctrl Pts',(6.94940340943504,1.42751594974962,-3.77262259695963));
#24794=CARTESIAN_POINT('Ctrl Pts',(6.80558863697834,-1.42751594974956,-3.77262259695965));
#24795=CARTESIAN_POINT('Ctrl Pts',(6.70971604449747,-2.85065573894359,-2.51505059188955));
#24796=CARTESIAN_POINT('Ctrl Pts',(6.66177386452166,-3.26701017360182,-1.72775056371106));
#24797=CARTESIAN_POINT('Ctrl Pts',(6.95623475686376,3.47674859222147,-1.83867022779103));
#24798=CARTESIAN_POINT('Ctrl Pts',(6.90829257688794,3.03366466604953,-2.67651404191289));
#24799=CARTESIAN_POINT('Ctrl Pts',(6.81241998440707,1.51916088562219,-4.01482077066858));
#24800=CARTESIAN_POINT('Ctrl Pts',(6.66860521195038,-1.51916088562212,-4.01482077066861));
#24801=CARTESIAN_POINT('Ctrl Pts',(6.57273261946951,-3.03366466604949,-2.67651404191294));
#24802=CARTESIAN_POINT('Ctrl Pts',(6.5247904394937,-3.47674859222144,-1.83867022779109));
#24803=CARTESIAN_POINT('Ctrl Pts',(6.90165719587644,2.84677340648494,-2.71056479661449));
#24804=CARTESIAN_POINT('Ctrl Pts',(6.87190753622973,2.44048989744138,-3.13623137002149));
#24805=CARTESIAN_POINT('Ctrl Pts',(6.79422746407799,1.13481420380713,-4.01482077066858));
#24806=CARTESIAN_POINT('Ctrl Pts',(6.68679773227946,-1.13481420380722,-4.01482077066861));
#24807=CARTESIAN_POINT('Ctrl Pts',(6.60911766012771,-2.44048989744134,-3.13623137002152));
#24808=CARTESIAN_POINT('Ctrl Pts',(6.579368000481,-2.8467734064849,-2.71056479661452));
#24809=CARTESIAN_POINT('Ctrl Pts',(8.61718818994175,2.84752960083224,-1.50590704659367));
#24810=CARTESIAN_POINT('Ctrl Pts',(8.56924596968449,2.48463487950633,-2.19211919452613));
#24811=CARTESIAN_POINT('Ctrl Pts',(8.47337333692217,1.24418392764402,-3.28820601234521));
#24812=CARTESIAN_POINT('Ctrl Pts',(8.32955848390258,-1.24418392764399,-3.28820601234522));
#24813=CARTESIAN_POINT('Ctrl Pts',(8.23368585114026,-2.48463487950632,-2.19211919452615));
#24814=CARTESIAN_POINT('Ctrl Pts',(8.18574363088299,-2.84752960083223,-1.5059070465937));
#24815=CARTESIAN_POINT('Ctrl Pts',(8.48020375253053,3.05726963691,-1.61682740302824));
#24816=CARTESIAN_POINT('Ctrl Pts',(8.43226153227327,2.66764523666483,-2.35358377028059));
#24817=CARTESIAN_POINT('Ctrl Pts',(8.33638889951095,1.33582658582575,-3.53040488095707));
#24818=CARTESIAN_POINT('Ctrl Pts',(8.19257404649136,-1.33582658582571,-3.53040488095709));
#24819=CARTESIAN_POINT('Ctrl Pts',(8.09670141372905,-2.66764523666481,-2.35358377028062));
#24820=CARTESIAN_POINT('Ctrl Pts',(8.04875919347178,-3.05726963690998,-1.61682740302827));
#24821=CARTESIAN_POINT('Ctrl Pts',(8.34321931511932,3.26700967298776,-1.7277477594628));
#24822=CARTESIAN_POINT('Ctrl Pts',(8.29527709486206,2.85065559382334,-2.51504834603505));
#24823=CARTESIAN_POINT('Ctrl Pts',(8.19940446209974,1.42746924400749,-3.77260374956895));
#24824=CARTESIAN_POINT('Ctrl Pts',(8.05558960908014,-1.42746924400744,-3.77260374956897));
#24825=CARTESIAN_POINT('Ctrl Pts',(7.95971697631782,-2.85065559382331,-2.51504834603509));
#24826=CARTESIAN_POINT('Ctrl Pts',(7.91177475606056,-3.26700967298774,-1.72774775946284));
#24827=CARTESIAN_POINT('Ctrl Pts',(8.20623487770811,3.47674970906552,-1.83866811589737));
#24828=CARTESIAN_POINT('Ctrl Pts',(8.15829265745084,3.03366595098184,-2.67651292178951));
#24829=CARTESIAN_POINT('Ctrl Pts',(8.06242002468851,1.51911190218921,-4.01480261818081));
#24830=CARTESIAN_POINT('Ctrl Pts',(7.91860517166893,-1.51911190218915,-4.01480261818084));
#24831=CARTESIAN_POINT('Ctrl Pts',(7.82273253890661,-3.0336659509818,-2.67651292178956));
#24832=CARTESIAN_POINT('Ctrl Pts',(7.77479031864935,-3.47674970906549,-1.83866811589743));
#24833=CARTESIAN_POINT('Ctrl Pts',(8.15165719587644,2.84676559888789,-2.71056162195416));
#24834=CARTESIAN_POINT('Ctrl Pts',(8.12190753622973,2.44047517949096,-3.13622513744625));
#24835=CARTESIAN_POINT('Ctrl Pts',(8.04422746407799,1.13477697746454,-4.0148026181808));
#24836=CARTESIAN_POINT('Ctrl Pts',(7.93679773227946,-1.13477697746461,-4.01480261818084));
#24837=CARTESIAN_POINT('Ctrl Pts',(7.85911766012771,-2.44047517949091,-3.13622513744629));
#24838=CARTESIAN_POINT('Ctrl Pts',(7.829368000481,-2.84676559888785,-2.71056162195421));
#24839=CARTESIAN_POINT('Ctrl Pts',(9.86719107484073,2.8475261883373,-1.50590321989084));
#24840=CARTESIAN_POINT('Ctrl Pts',(9.81924881778544,2.48463213407324,-2.19211508629638));
#24841=CARTESIAN_POINT('Ctrl Pts',(9.72337614822511,1.24414602360339,-3.28818693250078));
#24842=CARTESIAN_POINT('Ctrl Pts',(9.57956122160949,-1.24414602360339,-3.28818693250078));
#24843=CARTESIAN_POINT('Ctrl Pts',(9.48368855204915,-2.48463213407324,-2.19211508629638));
#24844=CARTESIAN_POINT('Ctrl Pts',(9.43574629499388,-2.8475261883373,-1.50590321989084));
#24845=CARTESIAN_POINT('Ctrl Pts',(9.73020571259453,3.05726770200041,-1.61682420880526));
#24846=CARTESIAN_POINT('Ctrl Pts',(9.68226345553925,2.66764379761156,-2.35358069044312));
#24847=CARTESIAN_POINT('Ctrl Pts',(9.58639078597891,1.33578664530418,-3.53038639224751));
#24848=CARTESIAN_POINT('Ctrl Pts',(9.4425758593633,-1.33578664530417,-3.53038639224751));
#24849=CARTESIAN_POINT('Ctrl Pts',(9.34670318980296,-2.66764379761156,-2.35358069044313));
#24850=CARTESIAN_POINT('Ctrl Pts',(9.29876093274769,-3.05726770200041,-1.61682420880527));
#24851=CARTESIAN_POINT('Ctrl Pts',(9.59322035034834,3.26700921566353,-1.72774519771967));
#24852=CARTESIAN_POINT('Ctrl Pts',(9.54527809329306,2.85065546114989,-2.51504629458986));
#24853=CARTESIAN_POINT('Ctrl Pts',(9.44940542373273,1.42742726700498,-3.77258585199426));
#24854=CARTESIAN_POINT('Ctrl Pts',(9.30559049711711,-1.42742726700496,-3.77258585199426));
#24855=CARTESIAN_POINT('Ctrl Pts',(9.20971782755677,-2.85065546114988,-2.51504629458988));
#24856=CARTESIAN_POINT('Ctrl Pts',(9.16177557050149,-3.26700921566353,-1.72774519771969));
#24857=CARTESIAN_POINT('Ctrl Pts',(9.45623498810215,3.47675072932665,-1.83866618663408));
#24858=CARTESIAN_POINT('Ctrl Pts',(9.40829273104687,3.03366712468821,-2.6765118987366));
#24859=CARTESIAN_POINT('Ctrl Pts',(9.31242006148653,1.51906788870579,-4.014785311741));
#24860=CARTESIAN_POINT('Ctrl Pts',(9.16860513487091,-1.51906788870575,-4.01478531174101));
#24861=CARTESIAN_POINT('Ctrl Pts',(9.07273246531058,-3.03366712468819,-2.67651189873662));
#24862=CARTESIAN_POINT('Ctrl Pts',(9.02479020825531,-3.47675072932664,-1.8386661866341));
#24863=CARTESIAN_POINT('Ctrl Pts',(9.40165719587644,2.84675858147378,-2.71055859525787));
#24864=CARTESIAN_POINT('Ctrl Pts',(9.37190753622973,2.44046195109913,-3.1362191953578));
#24865=CARTESIAN_POINT('Ctrl Pts',(9.29422746407799,1.13474351868581,-4.01478531174101));
#24866=CARTESIAN_POINT('Ctrl Pts',(9.18679773227947,-1.13474351868577,-4.01478531174101));
#24867=CARTESIAN_POINT('Ctrl Pts',(9.10911766012771,-2.4404619510991,-3.13621919535782));
#24868=CARTESIAN_POINT('Ctrl Pts',(9.079368000481,-2.84675858147374,-2.7105585952579));
#24869=CARTESIAN_POINT('Ctrl Pts',(11.102826855619,2.7325876658857,-1.7059759760899));
#24870=CARTESIAN_POINT('Ctrl Pts',(11.0564761776969,2.33512269759968,-2.34262495894918));
#24871=CARTESIAN_POINT('Ctrl Pts',(10.9637748218525,1.07966271388233,-3.32492883043245));
#24872=CARTESIAN_POINT('Ctrl Pts',(10.8247124167047,-1.31450087230183,-3.2393423413749));
#24873=CARTESIAN_POINT('Ctrl Pts',(10.7320006894791,-2.49670104301917,-2.16966721227558));
#24874=CARTESIAN_POINT('Ctrl Pts',(10.6856396401757,-2.84766280119442,-1.50605642114679));
#24875=CARTESIAN_POINT('Ctrl Pts',(10.965701366658,2.93405695958231,-1.83175484103065));
#24876=CARTESIAN_POINT('Ctrl Pts',(10.9193506887358,2.50728753844033,-2.515342929453));
#24877=CARTESIAN_POINT('Ctrl Pts',(10.8266493328915,1.15926450932041,-3.57007048550964));
#24878=CARTESIAN_POINT('Ctrl Pts',(10.6875869277437,-1.41141690746236,-3.47817384226539));
#24879=CARTESIAN_POINT('Ctrl Pts',(10.594875200518,-2.6807787953959,-2.32963328629069));
#24880=CARTESIAN_POINT('Ctrl Pts',(10.5485141512146,-3.05761639953827,-1.6170955388387));
#24881=CARTESIAN_POINT('Ctrl Pts',(10.828575877697,3.13552625327892,-1.9575337059714));
#24882=CARTESIAN_POINT('Ctrl Pts',(10.7822251997748,2.67945237928098,-2.68806089995681));
#24883=CARTESIAN_POINT('Ctrl Pts',(10.6895238439304,1.23886630475848,-3.81521214058682));
#24884=CARTESIAN_POINT('Ctrl Pts',(10.5504614387827,-1.50833294262289,-3.71700534315589));
#24885=CARTESIAN_POINT('Ctrl Pts',(10.4577497115571,-2.86485654777264,-2.48959936030581));
#24886=CARTESIAN_POINT('Ctrl Pts',(10.4113886622536,-3.26756999788213,-1.72813465653059));
#24887=CARTESIAN_POINT('Ctrl Pts',(10.6914503887359,3.33699554697554,-2.08331257091215));
#24888=CARTESIAN_POINT('Ctrl Pts',(10.6450997108137,2.85161722012163,-2.86077887046062));
#24889=CARTESIAN_POINT('Ctrl Pts',(10.5523983549694,1.31846810019657,-4.060353795664));
#24890=CARTESIAN_POINT('Ctrl Pts',(10.4133359498216,-1.60524897778342,-3.95583684404638));
#24891=CARTESIAN_POINT('Ctrl Pts',(10.320624222596,-3.04893430014939,-2.64956543432092));
#24892=CARTESIAN_POINT('Ctrl Pts',(10.2742631732926,-3.47752359622599,-1.83917377422248));
#24893=CARTESIAN_POINT('Ctrl Pts',(10.6516571958764,2.84853760141617,-2.71188542038896));
#24894=CARTESIAN_POINT('Ctrl Pts',(10.6455290770758,2.76494594567757,-2.79968926812744));
#24895=CARTESIAN_POINT('Ctrl Pts',(10.6394009582753,2.67728929704302,-2.88362738694732));
#24896=CARTESIAN_POINT('Ctrl Pts',(10.6332728394747,2.58595065464962,-2.96333396898109));
#24897=CARTESIAN_POINT('Ctrl Pts',(10.6271443176134,2.49460600469932,-3.04304579350383));
#24898=CARTESIAN_POINT('Ctrl Pts',(10.6210157957521,2.39957915068204,-3.11852529051356));
#24899=CARTESIAN_POINT('Ctrl Pts',(10.6148872738908,2.30128712085601,-3.18944612548672));
#24900=CARTESIAN_POINT('Ctrl Pts',(10.6087557427774,2.20294682727241,-3.26040178430055));
#24901=CARTESIAN_POINT('Ctrl Pts',(10.602624211664,2.1013384467335,-3.32679409720055));
#24902=CARTESIAN_POINT('Ctrl Pts',(10.5964926805506,1.99690932938873,-3.38833914037545));
#24903=CARTESIAN_POINT('Ctrl Pts',(10.5903597344877,1.89245611334498,-3.44989838605925));
#24904=CARTESIAN_POINT('Ctrl Pts',(10.5842267884249,1.78518117652743,-3.50660795423693));
#24905=CARTESIAN_POINT('Ctrl Pts',(10.5780938423621,1.67555727819519,-3.55822944840367));
#24906=CARTESIAN_POINT('Ctrl Pts',(10.571956787069,1.56585992905622,-3.6098855302876));
#24907=CARTESIAN_POINT('Ctrl Pts',(10.5658197317759,1.45381080309502,-3.65644657945933));
#24908=CARTESIAN_POINT('Ctrl Pts',(10.5596826764829,1.33990384989523,-3.69772182201906));
#24909=CARTESIAN_POINT('Ctrl Pts',(10.5574317208016,1.29812493619831,-3.71286079947636));
#24910=CARTESIAN_POINT('Ctrl Pts',(10.5551807651203,1.25609626319755,-3.72728916258503));
#24911=CARTESIAN_POINT('Ctrl Pts',(10.552929809439,1.21384274673912,-3.74099916949855));
#24912=CARTESIAN_POINT('Ctrl Pts',(10.5469118194765,1.10087684516881,-3.77765323811422));
#24913=CARTESIAN_POINT('Ctrl Pts',(10.5408938295139,0.986170791072762,-3.80921187257292));
#24914=CARTESIAN_POINT('Ctrl Pts',(10.5348758395513,0.870210701742948,-3.83552112946494));
#24915=CARTESIAN_POINT('Ctrl Pts',(10.5288613570294,0.754318196961284,-3.86181505263957));
#24916=CARTESIAN_POINT('Ctrl Pts',(10.5228468745075,0.637173487249866,-3.88286560447526));
#24917=CARTESIAN_POINT('Ctrl Pts',(10.5168323919856,0.519276265212455,-3.89856911704628));
#24918=CARTESIAN_POINT('Ctrl Pts',(10.5108202615803,0.401425149887673,-3.91426648835859));
#24919=CARTESIAN_POINT('Ctrl Pts',(10.504808131175,0.282822490030062,-3.92462093396961));
#24920=CARTESIAN_POINT('Ctrl Pts',(10.4987960007697,0.163976196133212,-3.92958023293859));
#24921=CARTESIAN_POINT('Ctrl Pts',(10.4927850693528,0.0451536035376617,
-3.93453854288355));
#24922=CARTESIAN_POINT('Ctrl Pts',(10.4867741379358,-0.0739121412827665,
-3.93410383408152));
#24923=CARTESIAN_POINT('Ctrl Pts',(10.4807632065188,-0.192710362649327,
-3.92827592158794));
#24924=CARTESIAN_POINT('Ctrl Pts',(10.4747504825599,-0.311544011269225,
-3.9224462711312));
#24925=CARTESIAN_POINT('Ctrl Pts',(10.468737758601,-0.430109591454027,-3.91122021779041));
#24926=CARTESIAN_POINT('Ctrl Pts',(10.4627250346421,-0.547898680884157,
-3.89464966787584));
#24927=CARTESIAN_POINT('Ctrl Pts',(10.4567115633265,-0.665702411011273,
-3.8780770583104));
#24928=CARTESIAN_POINT('Ctrl Pts',(10.4506980920108,-0.78272907699905,-3.85615868874641));
#24929=CARTESIAN_POINT('Ctrl Pts',(10.4446846206952,-0.898478527493888,
-3.82899795450878));
#24930=CARTESIAN_POINT('Ctrl Pts',(10.4386665678898,-1.01431616414513,-3.8018165272938));
#24931=CARTESIAN_POINT('Ctrl Pts',(10.4326485150844,-1.12887426660863,-3.76938484928543));
#24932=CARTESIAN_POINT('Ctrl Pts',(10.426630462279,-1.2416656642706,-3.73185682712661));
#24933=CARTESIAN_POINT('Ctrl Pts',(10.4223795667435,-1.32133669147319,-3.70534863469126));
#24934=CARTESIAN_POINT('Ctrl Pts',(10.418128671208,-1.40012652562735,-3.67629872628921));
#24935=CARTESIAN_POINT('Ctrl Pts',(10.4138777756725,-1.47786921651355,-3.64477592985929));
#24936=CARTESIAN_POINT('Ctrl Pts',(10.4076700973785,-1.59139861536529,-3.5987424817239));
#24937=CARTESIAN_POINT('Ctrl Pts',(10.4014624190846,-1.70282111743399,-3.54738213142518));
#24938=CARTESIAN_POINT('Ctrl Pts',(10.3952547407906,-1.81164015590211,-3.49090947254766));
#24939=CARTESIAN_POINT('Ctrl Pts',(10.3890514358049,-1.92038253137729,-3.43447659864811));
#24940=CARTESIAN_POINT('Ctrl Pts',(10.3828481308192,-2.02652479741291,-3.37293875908211));
#24941=CARTESIAN_POINT('Ctrl Pts',(10.3766448258335,-2.12959335724681,-3.30655729313288));
#24942=CARTESIAN_POINT('Ctrl Pts',(10.3704446314107,-2.23261023475236,-3.24020911326745));
#24943=CARTESIAN_POINT('Ctrl Pts',(10.364244436988,-2.33255619023717,-3.16902233521461));
#24944=CARTESIAN_POINT('Ctrl Pts',(10.3580442425652,-2.42898482509644,-3.09330272030579));
#24945=CARTESIAN_POINT('Ctrl Pts',(10.3518470240126,-2.52536717768228,-3.01761944808633));
#24946=CARTESIAN_POINT('Ctrl Pts',(10.34564980546,-2.61823530659864,-2.93740789034966));
#24947=CARTESIAN_POINT('Ctrl Pts',(10.3394525869073,-2.70717424489736,-2.85301535358021));
#24948=CARTESIAN_POINT('Ctrl Pts',(10.3360910580986,-2.75541698489033,-2.80723869729676));
#24949=CARTESIAN_POINT('Ctrl Pts',(10.3327295292898,-2.80250421571315,-2.76023260054377));
#24950=CARTESIAN_POINT('Ctrl Pts',(10.329368000481,-2.84837393363742,-2.71205732501636));
#24951=CARTESIAN_POINT('Origin',(11.0238490761436,0.781229937496414,-0.42649944676949));
#24952=CARTESIAN_POINT('Ctrl Pts',(4.24217562075336,-2.84754446865879,1.50592371916677));
#24953=CARTESIAN_POINT('Ctrl Pts',(4.19423356082101,-2.48464684011856,2.19213709545128));
#24954=CARTESIAN_POINT('Ctrl Pts',(4.0983610883836,-1.24435549640673,3.2882828077279));
#24955=CARTESIAN_POINT('Ctrl Pts',(3.95454655601384,1.24435549640671,3.2882828077279));
#24956=CARTESIAN_POINT('Ctrl Pts',(3.85867408357643,2.48464684011855,2.1921370954513));
#24957=CARTESIAN_POINT('Ctrl Pts',(3.81073202364408,2.84754446865879,1.50592371916679));
#24958=CARTESIAN_POINT('Ctrl Pts',(4.10519521274669,-3.05727806706812,1.61684131993722));
#24959=CARTESIAN_POINT('Ctrl Pts',(4.05725315281434,-2.66765150546796,2.35359719073546));
#24960=CARTESIAN_POINT('Ctrl Pts',(3.96138068037693,-1.33600750003101,3.53047863414712));
#24961=CARTESIAN_POINT('Ctrl Pts',(3.81756614800717,1.33600750003098,3.53047863414713));
#24962=CARTESIAN_POINT('Ctrl Pts',(3.72169367556977,2.66765150546794,2.35359719073547));
#24963=CARTESIAN_POINT('Ctrl Pts',(3.67375161563742,3.05727806706811,1.61684131993725));
#24964=CARTESIAN_POINT('Ctrl Pts',(3.96821480474003,-3.26701166547745,1.72775892070767));
#24965=CARTESIAN_POINT('Ctrl Pts',(3.92027274480768,-2.85065617081736,2.51505728601962));
#24966=CARTESIAN_POINT('Ctrl Pts',(3.82440027237027,-1.42765950365529,3.77267446056633));
#24967=CARTESIAN_POINT('Ctrl Pts',(3.68058574000051,1.42765950365525,3.77267446056634));
#24968=CARTESIAN_POINT('Ctrl Pts',(3.5847132675631,2.85065617081734,2.51505728601966));
#24969=CARTESIAN_POINT('Ctrl Pts',(3.53677120763075,3.26701166547743,1.7277589207077));
#24970=CARTESIAN_POINT('Ctrl Pts',(3.83123439673337,-3.47674526388677,1.83867652147811));
#24971=CARTESIAN_POINT('Ctrl Pts',(3.78329233680102,-3.03366083616676,2.67651738130379));
#24972=CARTESIAN_POINT('Ctrl Pts',(3.68741986436361,-1.51931150727957,4.01487028698555));
#24973=CARTESIAN_POINT('Ctrl Pts',(3.54360533199384,1.51931150727952,4.01487028698557));
#24974=CARTESIAN_POINT('Ctrl Pts',(3.44773285955643,3.03366083616673,2.67651738130383));
#24975=CARTESIAN_POINT('Ctrl Pts',(3.39979079962409,3.47674526388675,1.83867652147816));
#24976=CARTESIAN_POINT('Ctrl Pts',(3.77665719587644,-2.84679740187303,2.71057345644603));
#24977=CARTESIAN_POINT('Ctrl Pts',(3.74690753622973,-2.44053513068406,3.13624837122676));
#24978=CARTESIAN_POINT('Ctrl Pts',(3.66922746407795,-1.1349286129563,4.01487028698564));
#24979=CARTESIAN_POINT('Ctrl Pts',(3.56179773227949,1.13492861295628,4.01487028698554));
#24980=CARTESIAN_POINT('Ctrl Pts',(3.48411766012771,2.44053513068398,3.13624837122682));
#24981=CARTESIAN_POINT('Ctrl Pts',(3.454368000481,2.84679740187295,2.71057345644611));
#24982=CARTESIAN_POINT('Ctrl Pts',(5.49217968210715,-2.84753966457653,1.50591833191943));
#24983=CARTESIAN_POINT('Ctrl Pts',(5.44423757037064,-2.48464297555693,2.19213131100178));
#24984=CARTESIAN_POINT('Ctrl Pts',(5.34836504612908,-1.24429897509366,3.28825906217306));
#24985=CARTESIAN_POINT('Ctrl Pts',(5.204550410151,1.24429897509362,3.28825906217308));
#24986=CARTESIAN_POINT('Ctrl Pts',(5.10867788590944,2.4846429755569,2.19213131100181));
#24987=CARTESIAN_POINT('Ctrl Pts',(5.06073577417293,2.84753966457651,1.50591833191947));
#24988=CARTESIAN_POINT('Ctrl Pts',(5.35519797212004,-3.05727534312249,1.6168368231029));
#24989=CARTESIAN_POINT('Ctrl Pts',(5.30725586038353,-2.66764948005118,2.35359285399424));
#24990=CARTESIAN_POINT('Ctrl Pts',(5.21138333614197,-1.33594787926937,3.53045595032151));
#24991=CARTESIAN_POINT('Ctrl Pts',(5.0675687001639,1.33594787926931,3.53045595032154));
#24992=CARTESIAN_POINT('Ctrl Pts',(4.97169617592234,2.66764948005114,2.35359285399428));
#24993=CARTESIAN_POINT('Ctrl Pts',(4.92375406418583,3.05727534312247,1.61683682310294));
#24994=CARTESIAN_POINT('Ctrl Pts',(5.21821626213294,-3.26701102166844,1.72775531428636));
#24995=CARTESIAN_POINT('Ctrl Pts',(5.17027415039643,-2.85065598454542,2.51505439698671));
#24996=CARTESIAN_POINT('Ctrl Pts',(5.07440162615487,-1.42759678344509,3.77265283846997));
#24997=CARTESIAN_POINT('Ctrl Pts',(4.9305869901768,1.42759678344502,3.77265283847));
#24998=CARTESIAN_POINT('Ctrl Pts',(4.83471446593522,2.85065598454537,2.51505439698676));
#24999=CARTESIAN_POINT('Ctrl Pts',(4.78677235419872,3.26701102166841,1.72775531428642));
#25000=CARTESIAN_POINT('Ctrl Pts',(5.08123455214584,-3.4767467002144,1.83867380546982));
#25001=CARTESIAN_POINT('Ctrl Pts',(5.03329244040933,-3.03366248903967,2.67651593997917));
#25002=CARTESIAN_POINT('Ctrl Pts',(4.93741991616776,-1.51924568762079,4.01484972661843));
#25003=CARTESIAN_POINT('Ctrl Pts',(4.79360528018969,1.51924568762071,4.01484972661846));
#25004=CARTESIAN_POINT('Ctrl Pts',(4.69773275594812,3.03366248903961,2.67651593997923));
#25005=CARTESIAN_POINT('Ctrl Pts',(4.64979064421162,3.47674670021436,1.83867380546989));
#25006=CARTESIAN_POINT('Ctrl Pts',(5.02665719587644,-2.84678691836037,2.71056986067545));
#25007=CARTESIAN_POINT('Ctrl Pts',(4.99690753622973,-2.44051536841681,3.13624131191695));
#25008=CARTESIAN_POINT('Ctrl Pts',(4.919227464078,-1.1348786279445,4.01484972661831));
#25009=CARTESIAN_POINT('Ctrl Pts',(4.81179773227947,1.13487862794425,4.0148497266185));
#25010=CARTESIAN_POINT('Ctrl Pts',(4.73411766012771,2.44051536841673,3.13624131191701));
#25011=CARTESIAN_POINT('Ctrl Pts',(4.704368000481,2.8467869183603,2.71056986067553));
#25012=CARTESIAN_POINT('Ctrl Pts',(6.74218333694333,-2.84753534134887,1.50591348391091));
#25013=CARTESIAN_POINT('Ctrl Pts',(6.69424117858796,-2.48463949769956,2.19212610578529));
#25014=CARTESIAN_POINT('Ctrl Pts',(6.59836860772753,-1.24424897566079,3.2882368413454));
#25015=CARTESIAN_POINT('Ctrl Pts',(6.45455387851173,1.24424897566077,3.28823684134541));
#25016=CARTESIAN_POINT('Ctrl Pts',(6.3586813076513,2.48463949769954,2.1921261057853));
#25017=CARTESIAN_POINT('Ctrl Pts',(6.31073914929593,2.84753534134886,1.50591348391094));
#25018=CARTESIAN_POINT('Ctrl Pts',(6.60520045529636,-3.05727289182331,1.61683277637956));
#25019=CARTESIAN_POINT('Ctrl Pts',(6.55725829694099,-2.66764765724454,2.35358895159519));
#25020=CARTESIAN_POINT('Ctrl Pts',(6.46138572608056,-1.33589515421597,3.53043462216624));
#25021=CARTESIAN_POINT('Ctrl Pts',(6.31757099686476,1.33589515421593,3.53043462216624));
#25022=CARTESIAN_POINT('Ctrl Pts',(6.22169842600433,2.66764765724452,2.35358895159521));
#25023=CARTESIAN_POINT('Ctrl Pts',(6.17375626764897,3.05727289182329,1.6168327763796));
#25024=CARTESIAN_POINT('Ctrl Pts',(6.46821757364939,-3.26701044229775,1.72775206884821));
#25025=CARTESIAN_POINT('Ctrl Pts',(6.42027541529402,-2.85065581678953,2.5150517974051));
#25026=CARTESIAN_POINT('Ctrl Pts',(6.32440284443359,-1.42754133277114,3.77263240298708));
#25027=CARTESIAN_POINT('Ctrl Pts',(6.18058811521779,1.4275413327711,3.77263240298709));
#25028=CARTESIAN_POINT('Ctrl Pts',(6.08471554435736,2.8506558167895,2.51505179740513));
#25029=CARTESIAN_POINT('Ctrl Pts',(6.03677338600199,3.26701044229773,1.72775206884825));
#25030=CARTESIAN_POINT('Ctrl Pts',(6.33123469200243,-3.4767479927722,1.83867136131686));
#25031=CARTESIAN_POINT('Ctrl Pts',(6.28329253364706,-3.03366397633451,2.676514643215));
#25032=CARTESIAN_POINT('Ctrl Pts',(6.18741996278662,-1.51918751132632,4.01483018380791));
#25033=CARTESIAN_POINT('Ctrl Pts',(6.04360523357082,1.51918751132626,4.01483018380792));
#25034=CARTESIAN_POINT('Ctrl Pts',(5.94773266271039,3.03366397633447,2.67651464321504));
#25035=CARTESIAN_POINT('Ctrl Pts',(5.89979050435502,3.47674799277217,1.83867136131692));
#25036=CARTESIAN_POINT('Ctrl Pts',(6.27665719587644,-2.84677764951821,2.71056644286375));
#25037=CARTESIAN_POINT('Ctrl Pts',(6.24690753622973,-2.44049789590145,3.13623460198065));
#25038=CARTESIAN_POINT('Ctrl Pts',(6.16922746407796,-1.13483443443749,4.01483018380789));
#25039=CARTESIAN_POINT('Ctrl Pts',(6.06179773227948,1.13483443443743,4.01483018380793));
#25040=CARTESIAN_POINT('Ctrl Pts',(5.98411766012771,2.44049789590139,3.13623460198069));
#25041=CARTESIAN_POINT('Ctrl Pts',(5.954368000481,2.84677764951816,2.71056644286381));
#25042=CARTESIAN_POINT('Ctrl Pts',(7.99218664765765,-2.84753142517089,1.50590909237341));
#25043=CARTESIAN_POINT('Ctrl Pts',(7.94424444707283,-2.48463634719471,2.19212139087745));
#25044=CARTESIAN_POINT('Ctrl Pts',(7.84837183398294,-1.2442044285308,3.28821597875606));
#25045=CARTESIAN_POINT('Ctrl Pts',(7.70455702030822,1.24420442853079,3.28821597875607));
#25046=CARTESIAN_POINT('Ctrl Pts',(7.60868440721834,2.4846363471947,2.19212139087746));
#25047=CARTESIAN_POINT('Ctrl Pts',(7.56074220663351,2.84753142517089,1.50590909237343));
#25048=CARTESIAN_POINT('Ctrl Pts',(7.85520270466869,-3.05727067132307,1.61682911067984));
#25049=CARTESIAN_POINT('Ctrl Pts',(7.80726050408387,-2.6676460059526,2.35358541685185));
#25050=CARTESIAN_POINT('Ctrl Pts',(7.71138789099398,-1.33584819287788,3.53041451411671));
#25051=CARTESIAN_POINT('Ctrl Pts',(7.56757307731927,1.33584819287785,3.53041451411673));
#25052=CARTESIAN_POINT('Ctrl Pts',(7.47170046422939,2.66764600595259,2.35358541685187));
#25053=CARTESIAN_POINT('Ctrl Pts',(7.42375826364456,3.05727067132306,1.61682911067986));
#25054=CARTESIAN_POINT('Ctrl Pts',(7.71821876167974,-3.26700991747524,1.72774912898627));
#25055=CARTESIAN_POINT('Ctrl Pts',(7.67027656109492,-2.8506556647105,2.51504944282623));
#25056=CARTESIAN_POINT('Ctrl Pts',(7.57440394800502,-1.42749195722496,3.77261304947736));
#25057=CARTESIAN_POINT('Ctrl Pts',(7.43058913433032,1.42749195722492,3.77261304947737));
#25058=CARTESIAN_POINT('Ctrl Pts',(7.33471652124043,2.85065566471048,2.51504944282626));
#25059=CARTESIAN_POINT('Ctrl Pts',(7.2867743206556,3.26700991747522,1.7277491289863));
#25060=CARTESIAN_POINT('Ctrl Pts',(7.58123481869079,-3.47674916362741,1.83866914729269));
#25061=CARTESIAN_POINT('Ctrl Pts',(7.53329261810597,-3.0336653234684,2.67651346880062));
#25062=CARTESIAN_POINT('Ctrl Pts',(7.43742000501609,-1.51913572157204,4.01481158483801));
#25063=CARTESIAN_POINT('Ctrl Pts',(7.29360519134137,1.51913572157199,4.01481158483803));
#25064=CARTESIAN_POINT('Ctrl Pts',(7.19773257825148,3.03366532346837,2.67651346880066));
#25065=CARTESIAN_POINT('Ctrl Pts',(7.14979037766666,3.47674916362739,1.83866914729274));
#25066=CARTESIAN_POINT('Ctrl Pts',(7.52665719587644,-2.84676939580033,2.71056319011889));
#25067=CARTESIAN_POINT('Ctrl Pts',(7.49690753622974,-2.44048233697729,3.13622821610778));
#25068=CARTESIAN_POINT('Ctrl Pts',(7.41922746407797,-1.13479508100687,4.01481158483798));
#25069=CARTESIAN_POINT('Ctrl Pts',(7.31179773227947,1.13479508100694,4.01481158483804));
#25070=CARTESIAN_POINT('Ctrl Pts',(7.23411766012771,2.44048233697723,3.13622821610782));
#25071=CARTESIAN_POINT('Ctrl Pts',(7.204368000481,2.84676939580028,2.71056319011894));
#25072=CARTESIAN_POINT('Ctrl Pts',(9.24218966408072,-2.84752785710028,1.50590509120692));
#25073=CARTESIAN_POINT('Ctrl Pts',(9.19424742502024,-2.48463347664367,2.19211709526318));
#25074=CARTESIAN_POINT('Ctrl Pts',(9.0983747734547,-1.24416448608072,3.28819633497963));
#25075=CARTESIAN_POINT('Ctrl Pts',(8.95455988282867,1.24416448608072,3.28819633497963));
#25076=CARTESIAN_POINT('Ctrl Pts',(8.85868723126313,2.48463347664367,2.19211709526318));
#25077=CARTESIAN_POINT('Ctrl Pts',(8.81074499220265,2.84752785710028,1.50590509120692));
#25078=CARTESIAN_POINT('Ctrl Pts',(9.10520475409306,-3.05726864820132,1.61682577082915));
#25079=CARTESIAN_POINT('Ctrl Pts',(9.05726251503258,-2.66764450134284,2.35358219650886));
#25080=CARTESIAN_POINT('Ctrl Pts',(8.96138986346704,-1.33580609826714,3.53039551096818));
#25081=CARTESIAN_POINT('Ctrl Pts',(8.81757497284102,1.33580609826713,3.53039551096818));
#25082=CARTESIAN_POINT('Ctrl Pts',(8.72170232127548,2.66764450134284,2.35358219650887));
#25083=CARTESIAN_POINT('Ctrl Pts',(8.673760082215,3.05726864820131,1.61682577082916));
#25084=CARTESIAN_POINT('Ctrl Pts',(8.96821984410541,-3.26700943930236,1.72774645045138));
#25085=CARTESIAN_POINT('Ctrl Pts',(8.92027760504493,-2.85065552604202,2.51504729775454));
#25086=CARTESIAN_POINT('Ctrl Pts',(8.82440495347938,-1.42744771045355,3.77259468695673));
#25087=CARTESIAN_POINT('Ctrl Pts',(8.68059006285337,1.42744771045353,3.77259468695675));
#25088=CARTESIAN_POINT('Ctrl Pts',(8.58471741128782,2.85065552604201,2.51504729775456));
#25089=CARTESIAN_POINT('Ctrl Pts',(8.53677517222734,3.26700943930235,1.7277464504514));
#25090=CARTESIAN_POINT('Ctrl Pts',(8.83123493411776,-3.47675023040339,1.83866713007362));
#25091=CARTESIAN_POINT('Ctrl Pts',(8.78329269505728,-3.03366655074119,2.67651239900022));
#25092=CARTESIAN_POINT('Ctrl Pts',(8.68742004349173,-1.51908932263997,4.01479386294529));
#25093=CARTESIAN_POINT('Ctrl Pts',(8.54360515286572,1.51908932263994,4.0147938629453));
#25094=CARTESIAN_POINT('Ctrl Pts',(8.44773250130017,3.03366655074117,2.67651239900024));
#25095=CARTESIAN_POINT('Ctrl Pts',(8.39979026223969,3.47675023040338,1.83866713007365));
#25096=CARTESIAN_POINT('Ctrl Pts',(8.77665719587644,-2.84676199909996,2.71056009076467));
#25097=CARTESIAN_POINT('Ctrl Pts',(8.74690753622973,-2.44046839360025,3.13622213137543));
#25098=CARTESIAN_POINT('Ctrl Pts',(8.66922746407795,-1.13475981380474,4.01479386294536));
#25099=CARTESIAN_POINT('Ctrl Pts',(8.56179773227949,1.13475981380472,4.01479386294528));
#25100=CARTESIAN_POINT('Ctrl Pts',(8.48411766012771,2.4404683936002,3.13622213137546));
#25101=CARTESIAN_POINT('Ctrl Pts',(8.454368000481,2.84676199909991,2.71056009076472));
#25102=CARTESIAN_POINT('Ctrl Pts',(10.4921924265357,-2.84752458944047,1.50590142692301));
#25103=CARTESIAN_POINT('Ctrl Pts',(10.4442501522391,-2.48463084769168,2.19211316147804));
#25104=CARTESIAN_POINT('Ctrl Pts',(10.3483774654373,-1.244128467887,3.28817779179805));
#25105=CARTESIAN_POINT('Ctrl Pts',(10.204562504339,1.244128467887,3.28817779179805));
#25106=CARTESIAN_POINT('Ctrl Pts',(10.1086898175372,2.48463084769167,2.19211316147804));
#25107=CARTESIAN_POINT('Ctrl Pts',(10.0607475432405,2.84752458944047,1.50590142692301));
#25108=CARTESIAN_POINT('Ctrl Pts',(10.355206630966,-3.05726679541399,1.61682271217994));
#25109=CARTESIAN_POINT('Ctrl Pts',(10.3072643566693,-2.66764312332127,2.35357924747321));
#25110=CARTESIAN_POINT('Ctrl Pts',(10.2113916698675,-1.33576815041574,3.5303775137047));
#25111=CARTESIAN_POINT('Ctrl Pts',(10.0675767087691,1.33576815041572,3.53037751370471));
#25112=CARTESIAN_POINT('Ctrl Pts',(9.97170402196739,2.66764312332126,2.35357924747323));
#25113=CARTESIAN_POINT('Ctrl Pts',(9.92376174767071,3.05726679541398,1.61682271217996));
#25114=CARTESIAN_POINT('Ctrl Pts',(10.2182208353961,-3.2670090013875,1.72774399743689));
#25115=CARTESIAN_POINT('Ctrl Pts',(10.1702785610995,-2.85065539895085,2.51504533346838));
#25116=CARTESIAN_POINT('Ctrl Pts',(10.0744058742978,-1.42740783294447,3.77257723561135));
#25117=CARTESIAN_POINT('Ctrl Pts',(9.93059091319932,1.42740783294444,3.77257723561136));
#25118=CARTESIAN_POINT('Ctrl Pts',(9.83471822639758,2.85065539895083,2.5150453334684));
#25119=CARTESIAN_POINT('Ctrl Pts',(9.78677595210091,3.26700900138749,1.72774399743691));
#25120=CARTESIAN_POINT('Ctrl Pts',(10.0812350398263,-3.47675120736102,1.83866528269383));
#25121=CARTESIAN_POINT('Ctrl Pts',(10.0332927655296,-3.03366767458044,2.67651141946355));
#25122=CARTESIAN_POINT('Ctrl Pts',(9.93742007872794,-1.5190475154732,4.014776957518));
#25123=CARTESIAN_POINT('Ctrl Pts',(9.79360511762951,1.51904751547316,4.01477695751801));
#25124=CARTESIAN_POINT('Ctrl Pts',(9.69773243082778,3.03366767458041,2.67651141946358));
#25125=CARTESIAN_POINT('Ctrl Pts',(9.6497901565311,3.476751207361,1.83866528269385));
#25126=CARTESIAN_POINT('Ctrl Pts',(10.0266571958764,-2.84675533252353,2.71055713420083));
#25127=CARTESIAN_POINT('Ctrl Pts',(9.99690753622973,-2.44045582656577,3.13621632697281));
#25128=CARTESIAN_POINT('Ctrl Pts',(9.91922746407798,-1.13472802780763,4.01477695751801));
#25129=CARTESIAN_POINT('Ctrl Pts',(9.81179773227947,1.13472802780759,4.01477695751801));
#25130=CARTESIAN_POINT('Ctrl Pts',(9.73411766012771,2.44045582656573,3.13621632697284));
#25131=CARTESIAN_POINT('Ctrl Pts',(9.704368000481,2.84675533252349,2.71055713420087));
#25132=CARTESIAN_POINT('Origin',(3.02384907614375,0.,0.));
#25133=CARTESIAN_POINT('Ctrl Pts',(3.02384907614375,-0.0276919032690645,
3.22173788916774));
#25134=CARTESIAN_POINT('Ctrl Pts',(3.02384907614375,0.0782496652778502,
3.23412501519642));
#25135=CARTESIAN_POINT('Ctrl Pts',(3.02384907614376,0.184548923165627,3.24130018160313));
#25136=CARTESIAN_POINT('Ctrl Pts',(3.02384907614376,0.29078337533849,3.24328412261045));
#25137=CARTESIAN_POINT('Ctrl Pts',(3.02384907614375,0.398194429544279,3.24529003680042));
#25138=CARTESIAN_POINT('Ctrl Pts',(3.02384907614375,0.505540080276519,3.24198944432028));
#25139=CARTESIAN_POINT('Ctrl Pts',(3.02384907614375,0.612409252876001,3.23335728668128));
#25140=CARTESIAN_POINT('Ctrl Pts',(3.02384907614375,0.693096022241249,3.226839963719));
#25141=CARTESIAN_POINT('Ctrl Pts',(3.02384907614375,0.773511806360213,3.21728254875187));
#25142=CARTESIAN_POINT('Ctrl Pts',(3.02384907614375,0.85348463331301,3.204655194923));
#25143=CARTESIAN_POINT('Ctrl Pts',(3.02384907614375,0.948602940134049,3.18963643715743));
#25144=CARTESIAN_POINT('Ctrl Pts',(3.02384907614375,1.04309503128853,3.17027579824669));
#25145=CARTESIAN_POINT('Ctrl Pts',(3.02384907614375,1.13674268826725,3.14672432130043));
#25146=CARTESIAN_POINT('Ctrl Pts',(3.02384907614375,1.15921157599613,3.14107361408119));
#25147=CARTESIAN_POINT('Ctrl Pts',(3.02384907614375,1.18163183734145,3.13518149603407));
#25148=CARTESIAN_POINT('Ctrl Pts',(3.02384907614375,1.20400041713338,3.12904975582881));
#25149=CARTESIAN_POINT('Ctrl Pts',(3.02384907614375,1.22668855383874,3.12283041775225));
#25150=CARTESIAN_POINT('Ctrl Pts',(3.02384907614375,1.2493272800887,3.11636326663925));
#25151=CARTESIAN_POINT('Ctrl Pts',(3.02384907614375,1.27187893963434,3.10966082396874));
#25152=CARTESIAN_POINT('Ctrl Pts',(3.02384907614375,1.37566821122701,3.07881424076025));
#25153=CARTESIAN_POINT('Ctrl Pts',(3.02384907614375,1.47776583675392,3.04294833556332));
#25154=CARTESIAN_POINT('Ctrl Pts',(3.02384907614375,1.57787399167337,3.00235617549659));
#25155=CARTESIAN_POINT('Ctrl Pts',(3.02384907614375,1.67945971186073,2.96116488775727));
#25156=CARTESIAN_POINT('Ctrl Pts',(3.02384907614375,1.7789975445046,2.91510663424764));
#25157=CARTESIAN_POINT('Ctrl Pts',(3.02384907614375,1.87617830805873,2.86443319661672));
#25158=CARTESIAN_POINT('Ctrl Pts',(3.02384907614376,1.97420990098541,2.81331610689286));
#25159=CARTESIAN_POINT('Ctrl Pts',(3.02384907614375,2.06984379102712,2.75750242565906));
#25160=CARTESIAN_POINT('Ctrl Pts',(3.02384907614375,2.16275277600094,2.69719875918404));
#25161=CARTESIAN_POINT('Ctrl Pts',(3.02384907614375,2.22372524842834,2.65762386077722));
#25162=CARTESIAN_POINT('Ctrl Pts',(3.02384907614376,2.2835239426704,2.6161141717626));
#25163=CARTESIAN_POINT('Ctrl Pts',(3.02384907614376,2.34205147232849,2.57271690759623));
#25164=CARTESIAN_POINT('Ctrl Pts',(3.02384907614376,2.36251670760645,2.55754225001588));
#25165=CARTESIAN_POINT('Ctrl Pts',(3.02384907614375,2.38282647584896,2.54213672662517));
#25166=CARTESIAN_POINT('Ctrl Pts',(3.02384907614375,2.40297645819471,2.52650211691943));
#25167=CARTESIAN_POINT('Ctrl Pts',(3.02384907614375,2.41529317891841,2.51694542758514));
#25168=CARTESIAN_POINT('Ctrl Pts',(3.02384907614376,2.42754254591775,2.50730907271123));
#25169=CARTESIAN_POINT('Ctrl Pts',(3.02384907614376,2.43972290434689,2.49759447327991));
#25170=CARTESIAN_POINT('Ctrl Pts',(3.02384907614376,2.52887669079367,2.42648873955667));
#25171=CARTESIAN_POINT('Ctrl Pts',(3.02384907614376,2.61435347499606,2.35118026513924));
#25172=CARTESIAN_POINT('Ctrl Pts',(3.02384907614375,2.69583042064229,2.2719376795413));
#25173=CARTESIAN_POINT('Ctrl Pts',(3.02384907614375,2.74846100361106,2.22075039652654));
#25174=CARTESIAN_POINT('Ctrl Pts',(3.02384907614375,2.79942249209335,2.16792047495247));
#25175=CARTESIAN_POINT('Ctrl Pts',(3.02384907614375,2.84862442584919,2.11350930842726));
#25176=CARTESIAN_POINT('Origin',(3.02384907614375,0.,0.));
#25177=CARTESIAN_POINT('Origin',(11.0238490761438,0.,0.));
#25178=CARTESIAN_POINT('Origin',(11.0238490761438,0.,0.));
#25179=CARTESIAN_POINT('',(11.0238490761438,-1.74837398213582,3.52379982655521));
#25180=CARTESIAN_POINT('Ctrl Pts',(10.7710409564111,2.84675014301221,2.71055471688623));
#25181=CARTESIAN_POINT('Ctrl Pts',(10.8007906160578,2.44044604391822,3.13621158123827));
#25182=CARTESIAN_POINT('Ctrl Pts',(10.8784706882095,1.13470328440395,4.01476313548051));
#25183=CARTESIAN_POINT('Ctrl Pts',(10.9627400614538,-0.645450738027376,
4.01476313548051));
#25184=CARTESIAN_POINT('Ctrl Pts',(11.0172597750513,-1.6320315860502,3.5819951336082));
#25185=CARTESIAN_POINT('Ctrl Pts',(11.0238490761438,-1.74837398213582,3.52379982655521));
#25186=CARTESIAN_POINT('Origin',(11.0238490761438,0.,0.));
#25187=CARTESIAN_POINT('Origin',(11.0238490761438,0.,0.));
#25188=CARTESIAN_POINT('Ctrl Pts',(3.27104142627809,2.84862444224244,2.71179420072006));
#25189=CARTESIAN_POINT('Ctrl Pts',(3.27715668774982,2.76525344421169,2.79937188736806));
#25190=CARTESIAN_POINT('Ctrl Pts',(3.28327194922155,2.67782612651348,2.88311705070648));
#25191=CARTESIAN_POINT('Ctrl Pts',(3.28938721069328,2.58672031412161,2.96266215024775));
#25192=CARTESIAN_POINT('Ctrl Pts',(3.2955017508867,2.49562524741036,3.04219786766276));
#25193=CARTESIAN_POINT('Ctrl Pts',(3.30161629108012,2.40085282539269,3.11753427018141));
#25194=CARTESIAN_POINT('Ctrl Pts',(3.30773083127354,2.30281533001728,3.18834291691427));
#25195=CARTESIAN_POINT('Ctrl Pts',(3.31384732070615,2.20474658151039,3.25917413656108));
#25196=CARTESIAN_POINT('Ctrl Pts',(3.31996381013877,2.10341097249983,3.32547449962782));
#25197=CARTESIAN_POINT('Ctrl Pts',(3.32608029957138,1.9992515439133,3.38695767085452));
#25198=CARTESIAN_POINT('Ctrl Pts',(3.33219730689569,1.89508329600264,3.44844604794711));
#25199=CARTESIAN_POINT('Ctrl Pts',(3.33831431421999,1.78809106810152,3.50511623957712));
#25200=CARTESIAN_POINT('Ctrl Pts',(3.3444313215443,1.67874377661223,3.55672719399249));
#25201=CARTESIAN_POINT('Ctrl Pts',(3.35055243180748,1.56932314121,3.60837276608605));
#25202=CARTESIAN_POINT('Ctrl Pts',(3.35667354207066,1.45754461577093,3.65495216542421));
#25203=CARTESIAN_POINT('Ctrl Pts',(3.36279465233384,1.3438989665517,3.6962717118336));
#25204=CARTESIAN_POINT('Ctrl Pts',(3.36866578384342,1.23489446845073,3.73590381784961));
#25205=CARTESIAN_POINT('Ctrl Pts',(3.37453691535301,1.12417263389366,3.77069712601642));
#25206=CARTESIAN_POINT('Ctrl Pts',(3.3804080468626,1.01218020680333,3.80052367825219));
#25207=CARTESIAN_POINT('Ctrl Pts',(3.38643801180143,0.897158015992873,3.8311571368852));
#25208=CARTESIAN_POINT('Ctrl Pts',(3.39246797674025,0.780671237445417,3.85658409951363));
#25209=CARTESIAN_POINT('Ctrl Pts',(3.39849794167908,0.663216026372143,3.87667815305361));
#25210=CARTESIAN_POINT('Ctrl Pts',(3.40452465430829,0.545824165702508,3.89676136870576));
#25211=CARTESIAN_POINT('Ctrl Pts',(3.4105513669375,0.427465289416703,3.9115173384845));
#25212=CARTESIAN_POINT('Ctrl Pts',(3.41657807956671,0.308646188344926,3.92087063423676));
#25213=CARTESIAN_POINT('Ctrl Pts',(3.42260266217985,0.189869081409907,3.93022062426143));
#25214=CARTESIAN_POINT('Ctrl Pts',(3.42862724479299,0.0706324551248737,
3.93417171365013));
#25215=CARTESIAN_POINT('Ctrl Pts',(3.43465182740613,-0.0485516510990651,
3.93270031113172));
#25216=CARTESIAN_POINT('Ctrl Pts',(3.44067540027944,-0.167715781675204,
3.93122915522521));
#25217=CARTESIAN_POINT('Ctrl Pts',(3.44669897315274,-0.286827026949468,
3.92433732371218));
#25218=CARTESIAN_POINT('Ctrl Pts',(3.45272254602604,-0.405373546364642,
3.91205333398048));
#25219=CARTESIAN_POINT('Ctrl Pts',(3.45874784422619,-0.523954020958503,
3.89976582575604));
#25220=CARTESIAN_POINT('Ctrl Pts',(3.46477314242635,-0.641969065040415,
3.88208311012611));
#25221=CARTESIAN_POINT('Ctrl Pts',(3.4707984406265,-0.758912075489745,3.85908557325124));
#25222=CARTESIAN_POINT('Ctrl Pts',(3.47682460754683,-0.875871946640201,
3.83608472061945));
#25223=CARTESIAN_POINT('Ctrl Pts',(3.48285077446715,-0.991759101557666,
3.80776760026451));
#25224=CARTESIAN_POINT('Ctrl Pts',(3.48887694138748,-1.10607806193011,3.77426553397041));
#25225=CARTESIAN_POINT('Ctrl Pts',(3.49490708634063,-1.22047248728432,3.74074135207261));
#25226=CARTESIAN_POINT('Ctrl Pts',(3.50093723129378,-1.33329628462377,3.70202550216554));
#25227=CARTESIAN_POINT('Ctrl Pts',(3.50696737624693,-1.44406988066063,3.6582989462001));
#25228=CARTESIAN_POINT('Ctrl Pts',(3.50935832703864,-1.48799158058714,3.64096137895805));
#25229=CARTESIAN_POINT('Ctrl Pts',(3.51174927783036,-1.5315911802373,3.62283660276241));
#25230=CARTESIAN_POINT('Ctrl Pts',(3.51414022862207,-1.57483971028089,3.60393796934997));
#25231=CARTESIAN_POINT('Ctrl Pts',(3.52037156636177,-1.68755478512931,3.55468402066156));
#25232=CARTESIAN_POINT('Ctrl Pts',(3.52660290410147,-1.79799449153025,3.500122072768));
#25233=CARTESIAN_POINT('Ctrl Pts',(3.53283424184117,-1.90566526104715,3.44048381958673));
#25234=CARTESIAN_POINT('Ctrl Pts',(3.53906170132088,-2.01326901843035,3.38088268406157));
#25235=CARTESIAN_POINT('Ctrl Pts',(3.54528916080058,-2.11810698215066,3.3162117102347));
#25236=CARTESIAN_POINT('Ctrl Pts',(3.55151662028029,-2.21970999651663,3.24674860920339));
#25237=CARTESIAN_POINT('Ctrl Pts',(3.55774120404693,-2.32126609269433,3.17731758480752));
#25238=CARTESIAN_POINT('Ctrl Pts',(3.56396578781357,-2.41958993974689,3.10309903624059));
#25239=CARTESIAN_POINT('Ctrl Pts',(3.57019037158021,-2.51424092827549,3.02441424983159));
#25240=CARTESIAN_POINT('Ctrl Pts',(3.57641202806786,-2.60884740461503,2.94576646707299));
#25241=CARTESIAN_POINT('Ctrl Pts',(3.58263368455552,-2.69978420852058,2.86265685207649));
#25242=CARTESIAN_POINT('Ctrl Pts',(3.58885534104317,-2.78664338671542,2.77544728562356));
#25243=CARTESIAN_POINT('Ctrl Pts',(3.59034694463095,-2.80746733642786,2.75453933249758));
#25244=CARTESIAN_POINT('Ctrl Pts',(3.59183854821873,-2.8280570709332,2.73339590333766));
#25245=CARTESIAN_POINT('Ctrl Pts',(3.59333015180651,-2.84840726832521,2.71202231439052));
#25246=CARTESIAN_POINT('Origin',(11.0238490761438,0.,0.));
#25247=CARTESIAN_POINT('Ctrl Pts',(3.89604095641107,-2.84679354424148,-2.71057216472783));
#25248=CARTESIAN_POINT('Ctrl Pts',(3.92579061605778,-2.44052785873738,-3.13624583529209));
#25249=CARTESIAN_POINT('Ctrl Pts',(4.00347068820956,-1.13491021990779,-4.01486290103005));
#25250=CARTESIAN_POINT('Ctrl Pts',(4.11090042000803,1.13491021990785,-4.01486290102993));
#25251=CARTESIAN_POINT('Ctrl Pts',(4.1885804921598,2.44052785873742,-3.13624583529207));
#25252=CARTESIAN_POINT('Ctrl Pts',(4.21833015180651,2.84679354424151,-2.71057216472779));
#25253=CARTESIAN_POINT('Origin',(11.0238490761438,0.,0.));
#25254=CARTESIAN_POINT('Ctrl Pts',(4.52104095641107,2.84678837447174,2.71057037657591));
#25255=CARTESIAN_POINT('Ctrl Pts',(4.55079061605777,2.44051811330425,3.13624232474605));
#25256=CARTESIAN_POINT('Ctrl Pts',(4.62847068820955,1.13488557063109,4.01485267650142));
#25257=CARTESIAN_POINT('Ctrl Pts',(4.73590042000803,-1.13488557063111,4.01485267650135));
#25258=CARTESIAN_POINT('Ctrl Pts',(4.8135804921598,-2.44051811330426,3.13624232474605));
#25259=CARTESIAN_POINT('Ctrl Pts',(4.84333015180651,-2.84678837447173,2.71057037657592));
#25260=CARTESIAN_POINT('Origin',(11.0238490761438,0.,0.));
#25261=CARTESIAN_POINT('Ctrl Pts',(5.14604095641107,-2.84678351585588,-2.71056863339249));
#25262=CARTESIAN_POINT('Ctrl Pts',(5.17579061605778,-2.44050895442134,-3.13623890248327));
#25263=CARTESIAN_POINT('Ctrl Pts',(5.25347068820956,-1.13486240492507,-4.01484270909931));
#25264=CARTESIAN_POINT('Ctrl Pts',(5.36090042000802,1.13486240492515,-4.01484270909921));
#25265=CARTESIAN_POINT('Ctrl Pts',(5.4385804921598,2.44050895442139,-3.13623890248322));
#25266=CARTESIAN_POINT('Ctrl Pts',(5.46833015180651,2.84678351585592,-2.71056863339245));
#25267=CARTESIAN_POINT('Origin',(11.0238490761438,0.,0.));
#25268=CARTESIAN_POINT('Ctrl Pts',(5.77104095641107,2.84677894112342,2.71056693350226));
#25269=CARTESIAN_POINT('Ctrl Pts',(5.80079061605777,2.44050033068152,3.13623556521482));
#25270=CARTESIAN_POINT('Ctrl Pts',(5.87847068820954,1.13484059276487,4.01483298924472));
#25271=CARTESIAN_POINT('Ctrl Pts',(5.98590042000804,-1.13484059276507,4.01483298924472));
#25272=CARTESIAN_POINT('Ctrl Pts',(6.0635804921598,-2.44050033068153,3.13623556521481));
#25273=CARTESIAN_POINT('Ctrl Pts',(6.0933301518065,-2.84677894112342,2.71056693350226));
#25274=CARTESIAN_POINT('Origin',(11.0238490761438,0.,0.));
#25275=CARTESIAN_POINT('Ctrl Pts',(6.39604095641106,-2.8467746261001,-2.7105652753122));
#25276=CARTESIAN_POINT('Ctrl Pts',(6.42579061605777,-2.44049219651438,-3.13623230981321));
#25277=CARTESIAN_POINT('Ctrl Pts',(6.50347068820954,-1.13482001888854,-4.01482350782885));
#25278=CARTESIAN_POINT('Ctrl Pts',(6.61090042000804,1.13482001888872,-4.01482350782888));
#25279=CARTESIAN_POINT('Ctrl Pts',(6.6885804921598,2.44049219651441,-3.13623230981319));
#25280=CARTESIAN_POINT('Ctrl Pts',(6.71833015180651,2.84677462610012,-2.71056527531218));
#25281=CARTESIAN_POINT('Origin',(11.0238490761438,0.,0.));
#25282=CARTESIAN_POINT('Ctrl Pts',(7.02104095641106,2.84677054928067,2.71056365730649));
#25283=CARTESIAN_POINT('Ctrl Pts',(7.05079061605777,2.4404845113808,3.13622913330255));
#25284=CARTESIAN_POINT('Ctrl Pts',(7.12847068820954,1.13480058075977,4.01481425618423));
#25285=CARTESIAN_POINT('Ctrl Pts',(7.23590042000803,-1.13480058075978,4.01481425618427));
#25286=CARTESIAN_POINT('Ctrl Pts',(7.3135804921598,-2.4404845113808,3.13622913330254));
#25287=CARTESIAN_POINT('Ctrl Pts',(7.34333015180651,-2.84677054928066,2.7105636573065));
#25288=CARTESIAN_POINT('Origin',(11.0238490761438,0.,0.));
#25289=CARTESIAN_POINT('Ctrl Pts',(7.64604095641107,-2.84676669147043,-2.71056207804189));
#25290=CARTESIAN_POINT('Ctrl Pts',(7.67579061605778,-2.44047723909725,-3.1362260328494));
#25291=CARTESIAN_POINT('Ctrl Pts',(7.75347068820955,-1.13478218685908,-4.01480522605852));
#25292=CARTESIAN_POINT('Ctrl Pts',(7.86090042000803,1.13478218685912,-4.01480522605852));
#25293=CARTESIAN_POINT('Ctrl Pts',(7.9385804921598,2.4404772390973,-3.13622603284936));
#25294=CARTESIAN_POINT('Ctrl Pts',(7.96833015180651,2.84676669147048,-2.71056207804184));
#25295=CARTESIAN_POINT('Origin',(11.0238490761438,0.,0.));
#25296=CARTESIAN_POINT('Ctrl Pts',(8.27104095641106,2.84676303548313,2.71056053614337));
#25297=CARTESIAN_POINT('Ctrl Pts',(8.30079061605777,2.44047034726616,3.1362230057544));
#25298=CARTESIAN_POINT('Ctrl Pts',(8.37847068820953,1.13476475524287,4.01479640958965));
#25299=CARTESIAN_POINT('Ctrl Pts',(8.48590042000803,-1.13476475524271,4.01479640958985));
#25300=CARTESIAN_POINT('Ctrl Pts',(8.56358049215979,-2.44047034726616,3.1362230057544));
#25301=CARTESIAN_POINT('Ctrl Pts',(8.59333015180651,-2.84676303548312,2.71056053614338));
#25302=CARTESIAN_POINT('Origin',(11.0238490761438,0.,0.));
#25303=CARTESIAN_POINT('Ctrl Pts',(8.89604095641106,-2.84675956588473,-2.71055903030038));
#25304=CARTESIAN_POINT('Ctrl Pts',(8.92579061605777,-2.44046380679322,-3.1362200494445));
#25305=CARTESIAN_POINT('Ctrl Pts',(9.00347068820953,-1.13474821232218,-4.01478779928378));
#25306=CARTESIAN_POINT('Ctrl Pts',(9.11090042000803,1.13474821232205,-4.01478779928393));
#25307=CARTESIAN_POINT('Ctrl Pts',(9.18858049215979,2.44046380679323,-3.1362200494445));
#25308=CARTESIAN_POINT('Ctrl Pts',(9.21833015180651,2.84675956588473,-2.71055903030039));
#25309=CARTESIAN_POINT('Origin',(11.0238490761438,0.,0.));
#25310=CARTESIAN_POINT('Ctrl Pts',(9.52104095641107,2.84675626877589,2.71055755926284));
#25311=CARTESIAN_POINT('Ctrl Pts',(9.55079061605777,2.44045759147703,3.13621716146554));
#25312=CARTESIAN_POINT('Ctrl Pts',(9.62847068820954,1.1347324918254,4.01477938799309));
#25313=CARTESIAN_POINT('Ctrl Pts',(9.73590042000802,-1.13473249182541,4.01477938799308));
#25314=CARTESIAN_POINT('Ctrl Pts',(9.81358049215979,-2.44045759147703,3.13621716146554));
#25315=CARTESIAN_POINT('Ctrl Pts',(9.84333015180651,-2.84675626877588,2.71055755926285));
#25316=CARTESIAN_POINT('Origin',(11.0238490761438,0.,0.));
#25317=CARTESIAN_POINT('Ctrl Pts',(10.1460409564111,-2.84675313160574,-2.7105561218378));
#25318=CARTESIAN_POINT('Ctrl Pts',(10.1757906160578,-2.44045167765816,-3.13621433947552));
#25319=CARTESIAN_POINT('Ctrl Pts',(10.2534706882095,-1.13471753391067,-4.01477116889627));
#25320=CARTESIAN_POINT('Ctrl Pts',(10.360900420008,1.13471753391068,-4.01477116889624));
#25321=CARTESIAN_POINT('Ctrl Pts',(10.4385804921598,2.44045167765817,-3.13621433947552));
#25322=CARTESIAN_POINT('Ctrl Pts',(10.4683301518065,2.84675313160573,-2.71055612183781));
#25323=CARTESIAN_POINT('Ctrl Pts',(4.27290740952806,3.47674578943201,-1.83867552770464));
#25324=CARTESIAN_POINT('Ctrl Pts',(4.22496533064083,3.03366144096162,-2.67651685389203));
#25325=CARTESIAN_POINT('Ctrl Pts',(4.12909283924855,1.51928728527458,-4.01486290102995));
#25326=CARTESIAN_POINT('Ctrl Pts',(3.98527826896903,-1.51928728527452,-4.01486290102998));
#25327=CARTESIAN_POINT('Ctrl Pts',(3.88940577757674,-3.03366144096159,-2.67651685389207));
#25328=CARTESIAN_POINT('Ctrl Pts',(3.84146369868952,-3.47674578943198,-1.8386755277047));
#25329=CARTESIAN_POINT('Ctrl Pts',(4.13592652513338,3.26701142991145,-1.72775760113624));
#25330=CARTESIAN_POINT('Ctrl Pts',(4.08798444624615,2.85065610267767,-2.51505622890088));
#25331=CARTESIAN_POINT('Ctrl Pts',(3.99211195485387,1.42763642409474,-3.77266667786349));
#25332=CARTESIAN_POINT('Ctrl Pts',(3.84829738457435,-1.4276364240947,-3.7726666778635));
#25333=CARTESIAN_POINT('Ctrl Pts',(3.75242489318206,-2.85065610267764,-2.51505622890092));
#25334=CARTESIAN_POINT('Ctrl Pts',(3.70448281429483,-3.26701142991143,-1.72775760113627));
#25335=CARTESIAN_POINT('Ctrl Pts',(3.99894564073869,3.05727707039089,-1.61683967456782));
#25336=CARTESIAN_POINT('Ctrl Pts',(3.95100356185146,2.66765076439372,-2.35359560390975));
#25337=CARTESIAN_POINT('Ctrl Pts',(3.85513107045918,1.33598556291491,-3.53047045469701));
#25338=CARTESIAN_POINT('Ctrl Pts',(3.71131650017966,-1.33598556291488,-3.53047045469702));
#25339=CARTESIAN_POINT('Ctrl Pts',(3.61544400878737,-2.6676507643937,-2.35359560390977));
#25340=CARTESIAN_POINT('Ctrl Pts',(3.56750192990014,-3.05727707039087,-1.61683967456785));
#25341=CARTESIAN_POINT('Ctrl Pts',(3.86196475634401,2.84754271087033,-1.50592174799941));
#25342=CARTESIAN_POINT('Ctrl Pts',(3.81402267745678,2.48464542610977,-2.19213497891861));
#25343=CARTESIAN_POINT('Ctrl Pts',(3.71815018606449,1.24433470173507,-3.28827423153054));
#25344=CARTESIAN_POINT('Ctrl Pts',(3.57433561578498,-1.24433470173505,-3.28827423153055));
#25345=CARTESIAN_POINT('Ctrl Pts',(3.47846312439269,-2.48464542610976,-2.19213497891862));
#25346=CARTESIAN_POINT('Ctrl Pts',(3.43052104550547,-2.84754271087032,-1.50592174799943));
#25347=CARTESIAN_POINT('Ctrl Pts',(5.52290755913492,3.47674717210332,-1.83867291315533));
#25348=CARTESIAN_POINT('Ctrl Pts',(5.47496543037874,3.03366303203899,-2.67651546652179));
#25349=CARTESIAN_POINT('Ctrl Pts',(5.3790928891175,1.51922432968233,-4.01484270909923));
#25350=CARTESIAN_POINT('Ctrl Pts',(5.23527821910008,-1.51922432968225,-4.01484270909927));
#25351=CARTESIAN_POINT('Ctrl Pts',(5.13940567783883,-3.03366303203894,-2.67651546652185));
#25352=CARTESIAN_POINT('Ctrl Pts',(5.09146354908265,-3.47674717210328,-1.83867291315541));
#25353=CARTESIAN_POINT('Ctrl Pts',(5.3859254213967,3.2670108101514,-1.72775412943732));
#25354=CARTESIAN_POINT('Ctrl Pts',(5.33798329264052,2.85065592331588,-2.51505344789686));
#25355=CARTESIAN_POINT('Ctrl Pts',(5.24211075137927,1.4275764277431,-3.77264548798055));
#25356=CARTESIAN_POINT('Ctrl Pts',(5.09829608136185,-1.42757642774303,-3.77264548798058));
#25357=CARTESIAN_POINT('Ctrl Pts',(5.00242354010061,-2.85065592331583,-2.51505344789692));
#25358=CARTESIAN_POINT('Ctrl Pts',(4.95448141134442,-3.26701081015137,-1.72775412943738));
#25359=CARTESIAN_POINT('Ctrl Pts',(5.24894328365846,3.05727444819947,-1.61683534571931));
#25360=CARTESIAN_POINT('Ctrl Pts',(5.20100115490228,2.66764881459276,-2.35359142927193));
#25361=CARTESIAN_POINT('Ctrl Pts',(5.10512861364104,1.33592852580386,-3.53044826686187));
#25362=CARTESIAN_POINT('Ctrl Pts',(4.96131394362362,-1.33592852580381,-3.53044826686189));
#25363=CARTESIAN_POINT('Ctrl Pts',(4.86544140236237,-2.66764881459272,-2.35359142927197));
#25364=CARTESIAN_POINT('Ctrl Pts',(4.81749927360619,-3.05727444819945,-1.61683534571936));
#25365=CARTESIAN_POINT('Ctrl Pts',(5.11196114592024,2.84753808624755,-1.5059165620013));
#25366=CARTESIAN_POINT('Ctrl Pts',(5.06401901716406,2.48464170586964,-2.192129410647));
#25367=CARTESIAN_POINT('Ctrl Pts',(4.96814647590282,1.24428062386463,-3.28825104574319));
#25368=CARTESIAN_POINT('Ctrl Pts',(4.82433180588539,-1.24428062386459,-3.2882510457432));
#25369=CARTESIAN_POINT('Ctrl Pts',(4.72845926462415,-2.48464170586961,-2.19212941064703));
#25370=CARTESIAN_POINT('Ctrl Pts',(4.68051713586797,-2.84753808624753,-1.50591656200134));
#25371=CARTESIAN_POINT('Ctrl Pts',(6.77290769409362,3.47674841939408,-1.83867055459827));
#25372=CARTESIAN_POINT('Ctrl Pts',(6.72496552035121,3.03366446720085,-2.67651421526794));
#25373=CARTESIAN_POINT('Ctrl Pts',(6.62909293410373,1.51916853850403,-4.01482350782886));
#25374=CARTESIAN_POINT('Ctrl Pts',(6.48527817411384,-1.51916853850395,-4.01482350782889));
#25375=CARTESIAN_POINT('Ctrl Pts',(6.38940558786636,-3.0336644672008,-2.676514215268));
#25376=CARTESIAN_POINT('Ctrl Pts',(6.34146341412395,-3.47674841939404,-1.83867055459834));
#25377=CARTESIAN_POINT('Ctrl Pts',(6.63592442572804,3.26701025106974,-1.72775099765761));
#25378=CARTESIAN_POINT('Ctrl Pts',(6.58798225198562,2.85065576139054,-2.51505093944593));
#25379=CARTESIAN_POINT('Ctrl Pts',(6.49210966573815,1.42752324577464,-3.7726254459903));
#25380=CARTESIAN_POINT('Ctrl Pts',(6.34829490574825,-1.42752324577457,-3.77262544599032));
#25381=CARTESIAN_POINT('Ctrl Pts',(6.25242231950077,-2.85065576139049,-2.51505093944599));
#25382=CARTESIAN_POINT('Ctrl Pts',(6.20448014575836,-3.26701025106971,-1.72775099765767));
#25383=CARTESIAN_POINT('Ctrl Pts',(6.49894115736244,3.0572720827454,-1.61683144071695));
#25384=CARTESIAN_POINT('Ctrl Pts',(6.45099898362002,2.66764705558023,-2.35358766362393));
#25385=CARTESIAN_POINT('Ctrl Pts',(6.35512639737254,1.33587795304525,-3.53042738415174));
#25386=CARTESIAN_POINT('Ctrl Pts',(6.21131163738265,-1.3358779530452,-3.53042738415176));
#25387=CARTESIAN_POINT('Ctrl Pts',(6.11543905113517,-2.66764705558019,-2.35358766362397));
#25388=CARTESIAN_POINT('Ctrl Pts',(6.06749687739276,-3.05727208274538,-1.616831440717));
#25389=CARTESIAN_POINT('Ctrl Pts',(6.36195788899684,2.84753391442106,-1.5059118837763));
#25390=CARTESIAN_POINT('Ctrl Pts',(6.31401571525443,2.48463834976992,-2.19212438780192));
#25391=CARTESIAN_POINT('Ctrl Pts',(6.21814312900695,1.24423266031586,-3.28822932231318));
#25392=CARTESIAN_POINT('Ctrl Pts',(6.07432836901706,-1.24423266031582,-3.2882293223132));
#25393=CARTESIAN_POINT('Ctrl Pts',(5.97845578276958,-2.4846383497699,-2.19212438780196));
#25394=CARTESIAN_POINT('Ctrl Pts',(5.93051360902717,-2.84753391442104,-1.50591188377634));
#25395=CARTESIAN_POINT('Ctrl Pts',(8.02290781660591,3.47674955165342,-1.83866841355563));
#25396=CARTESIAN_POINT('Ctrl Pts',(7.97496560202607,3.03366576988594,-2.67651307964991));
#25397=CARTESIAN_POINT('Ctrl Pts',(7.87909297494116,1.51911875599997,-4.01480522605851));
#25398=CARTESIAN_POINT('Ctrl Pts',(7.73527813327642,-1.51911875599992,-4.01480522605853));
#25399=CARTESIAN_POINT('Ctrl Pts',(7.6394055061915,-3.03366576988591,-2.67651307964995));
#25400=CARTESIAN_POINT('Ctrl Pts',(7.59146329161166,-3.4767495516534,-1.83866841355567));
#25401=CARTESIAN_POINT('Ctrl Pts',(7.88592352188379,3.26700974354634,-1.727748154704));
#25402=CARTESIAN_POINT('Ctrl Pts',(7.83798130730395,2.85065561428405,-2.51504866256101));
#25403=CARTESIAN_POINT('Ctrl Pts',(7.74210868021904,1.42747577981153,-3.77260645240789));
#25404=CARTESIAN_POINT('Ctrl Pts',(7.59829383855429,-1.4274757798115,-3.77260645240791));
#25405=CARTESIAN_POINT('Ctrl Pts',(7.50242121146939,-2.85065561428403,-2.51504866256103));
#25406=CARTESIAN_POINT('Ctrl Pts',(7.45447899688955,-3.26700974354632,-1.72774815470403));
#25407=CARTESIAN_POINT('Ctrl Pts',(7.74893922716167,3.05726993543926,-1.61682789585237));
#25408=CARTESIAN_POINT('Ctrl Pts',(7.70099701258182,2.66764545868216,-2.35358424547209));
#25409=CARTESIAN_POINT('Ctrl Pts',(7.60512438549692,1.3358328036231,-3.53040767875727));
#25410=CARTESIAN_POINT('Ctrl Pts',(7.46130954383218,-1.33583280362307,-3.53040767875728));
#25411=CARTESIAN_POINT('Ctrl Pts',(7.36543691674726,-2.66764545868214,-2.35358424547211));
#25412=CARTESIAN_POINT('Ctrl Pts',(7.31749470216742,-3.05726993543925,-1.61682789585239));
#25413=CARTESIAN_POINT('Ctrl Pts',(7.61195493243955,2.84753012733218,-1.50590763700073));
#25414=CARTESIAN_POINT('Ctrl Pts',(7.56401271785971,2.48463530308027,-2.19211982838319));
#25415=CARTESIAN_POINT('Ctrl Pts',(7.46814009077479,1.24418982743467,-3.28820890510665));
#25416=CARTESIAN_POINT('Ctrl Pts',(7.32432524911005,-1.24418982743466,-3.28820890510666));
#25417=CARTESIAN_POINT('Ctrl Pts',(7.22845262202514,-2.48463530308026,-2.1921198283832));
#25418=CARTESIAN_POINT('Ctrl Pts',(7.1805104074453,-2.84753012733217,-1.50590763700075));
#25419=CARTESIAN_POINT('Ctrl Pts',(9.27290792843865,3.47675058521116,-1.83866645914951));
#25420=CARTESIAN_POINT('Ctrl Pts',(9.22496567658123,3.03366695890456,-2.67651204323431));
#25421=CARTESIAN_POINT('Ctrl Pts',(9.12909301221873,1.51907406221497,-4.01478779928389));
#25422=CARTESIAN_POINT('Ctrl Pts',(8.98527809599884,-1.51907406221493,-4.0147877992839));
#25423=CARTESIAN_POINT('Ctrl Pts',(8.88940543163634,-3.03366695890454,-2.67651204323434));
#25424=CARTESIAN_POINT('Ctrl Pts',(8.84146317977892,-3.47675058521115,-1.83866645914954));
#25425=CARTESIAN_POINT('Ctrl Pts',(9.13592269682874,3.26700928026235,-1.72774555957507));
#25426=CARTESIAN_POINT('Ctrl Pts',(9.08798044497131,2.85065547989676,-2.51504658435239));
#25427=CARTESIAN_POINT('Ctrl Pts',(8.99210778060883,1.42743315547921,-3.77258842044544));
#25428=CARTESIAN_POINT('Ctrl Pts',(8.84829286438891,-1.42743315547918,-3.77258842044545));
#25429=CARTESIAN_POINT('Ctrl Pts',(8.75242020002643,-2.85065547989675,-2.51504658435239));
#25430=CARTESIAN_POINT('Ctrl Pts',(8.70447794816901,-3.26700928026234,-1.72774555957508));
#25431=CARTESIAN_POINT('Ctrl Pts',(8.99893746521881,3.05726797531354,-1.61682466000062));
#25432=CARTESIAN_POINT('Ctrl Pts',(8.95099521336139,2.66764400088895,-2.35358112547045));
#25433=CARTESIAN_POINT('Ctrl Pts',(8.85512254899891,1.33579224874343,-3.530389041607));
#25434=CARTESIAN_POINT('Ctrl Pts',(8.71130763277899,-1.33579224874342,-3.530389041607));
#25435=CARTESIAN_POINT('Ctrl Pts',(8.61543496841651,-2.66764400088894,-2.35358112547046));
#25436=CARTESIAN_POINT('Ctrl Pts',(8.56749271655908,-3.05726797531354,-1.61682466000063));
#25437=CARTESIAN_POINT('Ctrl Pts',(8.8619522336089,2.84752667036473,-1.50590376042617));
#25438=CARTESIAN_POINT('Ctrl Pts',(8.81400998175148,2.48463252188115,-2.19211566658852));
#25439=CARTESIAN_POINT('Ctrl Pts',(8.718137317389,1.24415134200766,-3.28818966276855));
#25440=CARTESIAN_POINT('Ctrl Pts',(8.57432240116908,-1.24415134200766,-3.28818966276855));
#25441=CARTESIAN_POINT('Ctrl Pts',(8.47844973680659,-2.48463252188115,-2.19211566658852));
#25442=CARTESIAN_POINT('Ctrl Pts',(8.43050748494917,-2.84752667036473,-1.50590376042617));
#25443=CARTESIAN_POINT('Ctrl Pts',(10.5229080310278,3.47675153333854,-1.83866466628547));
#25444=CARTESIAN_POINT('Ctrl Pts',(10.474965744974,3.03366804954435,-2.67651109266735));
#25445=CARTESIAN_POINT('Ctrl Pts',(10.3790930464151,1.51903371577996,-4.01477116889625));
#25446=CARTESIAN_POINT('Ctrl Pts',(10.2352780618025,-1.51903371577993,-4.01477116889626));
#25447=CARTESIAN_POINT('Ctrl Pts',(10.1394053632436,-3.03366804954433,-2.67651109266738));
#25448=CARTESIAN_POINT('Ctrl Pts',(10.0914630771898,-3.47675153333853,-1.8386646662855));
#25449=CARTESIAN_POINT('Ctrl Pts',(10.3859219399691,3.26700885526974,-1.72774317894903));
#25450=CARTESIAN_POINT('Ctrl Pts',(10.3379796539154,2.85065535652278,-2.51504467809219));
#25451=CARTESIAN_POINT('Ctrl Pts',(10.2421069553564,1.42739466807426,-3.77257127375762));
#25452=CARTESIAN_POINT('Ctrl Pts',(10.0982919707438,-1.42739466807423,-3.77257127375763));
#25453=CARTESIAN_POINT('Ctrl Pts',(10.0024192721849,-2.85065535652277,-2.5150446780922));
#25454=CARTESIAN_POINT('Ctrl Pts',(9.95447698613115,-3.26700885526973,-1.72774317894905));
#25455=CARTESIAN_POINT('Ctrl Pts',(10.2489358489105,3.05726617720095,-1.61682169161259));
#25456=CARTESIAN_POINT('Ctrl Pts',(10.2009935628567,2.6676426635012,-2.35357826351702));
#25457=CARTESIAN_POINT('Ctrl Pts',(10.1051208642979,1.33575562036855,-3.53037137861899));
#25458=CARTESIAN_POINT('Ctrl Pts',(9.96130587968519,-1.33575562036854,-3.53037137861899));
#25459=CARTESIAN_POINT('Ctrl Pts',(9.86543318112631,-2.66764266350119,-2.35357826351704));
#25460=CARTESIAN_POINT('Ctrl Pts',(9.81749089507251,-3.05726617720095,-1.6168216916126));
#25461=CARTESIAN_POINT('Ctrl Pts',(10.1119497578518,2.84752349913215,-1.50590020427614));
#25462=CARTESIAN_POINT('Ctrl Pts',(10.0640074717981,2.48462997047963,-2.19211184894187));
#25463=CARTESIAN_POINT('Ctrl Pts',(9.96813477323921,1.24411657266284,-3.28817148348035));
#25464=CARTESIAN_POINT('Ctrl Pts',(9.82431978862655,-1.24411657266284,-3.28817148348035));
#25465=CARTESIAN_POINT('Ctrl Pts',(9.72844709006768,-2.48462997047963,-2.19211184894187));
#25466=CARTESIAN_POINT('Ctrl Pts',(9.68050480401388,-2.84752349913215,-1.50590020427614));
#25467=CARTESIAN_POINT('Ctrl Pts',(3.64838128925859,-3.47740286631016,1.83922164452567));
#25468=CARTESIAN_POINT('Ctrl Pts',(3.60379518879799,-3.06521053407891,2.61855938315106));
#25469=CARTESIAN_POINT('Ctrl Pts',(3.51463169441755,-1.69992623500153,3.88752819359771));
#25470=CARTESIAN_POINT('Ctrl Pts',(3.38089080611729,1.09279645395022,4.09974510230776));
#25471=CARTESIAN_POINT('Ctrl Pts',(3.29173601827763,2.63403351313429,3.0518682259016));
#25472=CARTESIAN_POINT('Ctrl Pts',(3.24715862435781,3.1592487603224,2.34397402547678));
#25473=CARTESIAN_POINT('Ctrl Pts',(3.51131387403993,-3.26754097150884,1.72822428410498));
#25474=CARTESIAN_POINT('Ctrl Pts',(3.46672777357933,-2.88022452142018,2.46052884860418));
#25475=CARTESIAN_POINT('Ctrl Pts',(3.37756427919888,-1.59733537785462,3.65291516077772));
#25476=CARTESIAN_POINT('Ctrl Pts',(3.24382339089863,1.02684598940094,3.85232474048881));
#25477=CARTESIAN_POINT('Ctrl Pts',(3.15466860305897,2.47506911203139,2.86768742396558));
#25478=CARTESIAN_POINT('Ctrl Pts',(3.11009120913914,2.9685875236238,2.20251476715576));
#25479=CARTESIAN_POINT('Ctrl Pts',(3.37424645882128,-3.05767907670752,1.61722692368431));
#25480=CARTESIAN_POINT('Ctrl Pts',(3.32966035836067,-2.69523850876146,2.30249831405731));
#25481=CARTESIAN_POINT('Ctrl Pts',(3.24049686398023,-1.4947445207077,3.41830212795774));
#25482=CARTESIAN_POINT('Ctrl Pts',(3.10675597567997,0.960895524851675,3.60490437866986));
#25483=CARTESIAN_POINT('Ctrl Pts',(3.01760118784032,2.31610471092849,2.68350662202955));
#25484=CARTESIAN_POINT('Ctrl Pts',(2.97302379392049,2.77792628692519,2.06105550883474));
#25485=CARTESIAN_POINT('Ctrl Pts',(3.23717904360261,-2.84781718190621,1.50622956326363));
#25486=CARTESIAN_POINT('Ctrl Pts',(3.192592943142,-2.51025249610272,2.14446777951043));
#25487=CARTESIAN_POINT('Ctrl Pts',(3.10342944876156,-1.39215366356079,3.18368909513775));
#25488=CARTESIAN_POINT('Ctrl Pts',(2.96968856046131,0.8949450603024,3.35748401685091));
#25489=CARTESIAN_POINT('Ctrl Pts',(2.88053377262165,2.15714030982559,2.49932582009352));
#25490=CARTESIAN_POINT('Ctrl Pts',(2.83595637870183,2.5872650502266,1.91959625051372));
#25491=CARTESIAN_POINT('Ctrl Pts',(4.89790748632074,-3.47674649915261,1.83867418566579));
#25492=CARTESIAN_POINT('Ctrl Pts',(4.84996538183595,-3.03366225767408,2.67651614172047));
#25493=CARTESIAN_POINT('Ctrl Pts',(4.7540928648461,-1.51925482848182,4.01485267650136));
#25494=CARTESIAN_POINT('Ctrl Pts',(4.61027824337146,1.51925482848179,4.01485267650137));
#25495=CARTESIAN_POINT('Ctrl Pts',(4.51440572638162,3.03366225767406,2.67651614172049));
#25496=CARTESIAN_POINT('Ctrl Pts',(4.46646362189683,3.47674649915259,1.83867418566581));
#25497=CARTESIAN_POINT('Ctrl Pts',(4.76092595858921,-3.26701111179121,1.72775581912512));
#25498=CARTESIAN_POINT('Ctrl Pts',(4.71298385410442,-2.85065601062904,2.51505480138416));
#25499=CARTESIAN_POINT('Ctrl Pts',(4.61711133711457,-1.42760549482174,3.77265593264611));
#25500=CARTESIAN_POINT('Ctrl Pts',(4.47329671563993,1.42760549482173,3.77265593264612));
#25501=CARTESIAN_POINT('Ctrl Pts',(4.37742419865009,2.85065601062903,2.51505480138416));
#25502=CARTESIAN_POINT('Ctrl Pts',(4.32948209416529,3.26701111179121,1.72775581912514));
#25503=CARTESIAN_POINT('Ctrl Pts',(4.62394443085768,-3.05727572442982,1.61683745258446));
#25504=CARTESIAN_POINT('Ctrl Pts',(4.57600232637288,-2.66764976358399,2.35359346104786));
#25505=CARTESIAN_POINT('Ctrl Pts',(4.48012980938304,-1.33595616116168,3.53045918879086));
#25506=CARTESIAN_POINT('Ctrl Pts',(4.33631518790839,1.33595616116167,3.53045918879086));
#25507=CARTESIAN_POINT('Ctrl Pts',(4.24044267091855,2.66764976358399,2.35359346104786));
#25508=CARTESIAN_POINT('Ctrl Pts',(4.19250056643376,3.05727572442982,1.61683745258447));
#25509=CARTESIAN_POINT('Ctrl Pts',(4.48696290312614,-2.84754033706844,1.50591908604379));
#25510=CARTESIAN_POINT('Ctrl Pts',(4.43902079864135,-2.48464351653895,2.19213212071155));
#25511=CARTESIAN_POINT('Ctrl Pts',(4.34314828165151,-1.24430682750162,3.28826244493561));
#25512=CARTESIAN_POINT('Ctrl Pts',(4.19933366017687,1.24430682750162,3.28826244493561));
#25513=CARTESIAN_POINT('Ctrl Pts',(4.10346114318702,2.48464351653896,2.19213212071155));
#25514=CARTESIAN_POINT('Ctrl Pts',(4.05551903870224,2.84754033706845,1.50591908604379));
#25515=CARTESIAN_POINT('Ctrl Pts',(6.14790762829603,-3.47674781129169,1.8386717044864));
#25516=CARTESIAN_POINT('Ctrl Pts',(6.09996547648614,-3.03366376752034,2.67651482526888));
#25517=CARTESIAN_POINT('Ctrl Pts',(6.0040929121712,-1.51919561710872,4.01483298924471));
#25518=CARTESIAN_POINT('Ctrl Pts',(5.86027819604637,1.51919561710867,4.01483298924473));
#25519=CARTESIAN_POINT('Ctrl Pts',(5.76440563173143,3.03366376752031,2.67651482526892));
#25520=CARTESIAN_POINT('Ctrl Pts',(5.71646347992155,3.47674781129167,1.83867170448645));
#25521=CARTESIAN_POINT('Ctrl Pts',(6.01092491115509,-3.26701052364405,1.72775252452145));
#25522=CARTESIAN_POINT('Ctrl Pts',(5.96298275934521,-2.85065584035111,2.51505216238105));
#25523=CARTESIAN_POINT('Ctrl Pts',(5.86711019503026,-1.42754905962654,3.77263533004504));
#25524=CARTESIAN_POINT('Ctrl Pts',(5.72329547890544,1.4275490596265,3.77263533004505));
#25525=CARTESIAN_POINT('Ctrl Pts',(5.62742291459049,2.85065584035108,2.51505216238109));
#25526=CARTESIAN_POINT('Ctrl Pts',(5.57948076278061,3.26701052364403,1.72775252452148));
#25527=CARTESIAN_POINT('Ctrl Pts',(5.87394219401415,-3.0572732359964,1.6168333445565));
#25528=CARTESIAN_POINT('Ctrl Pts',(5.82600004220427,-2.66764791318189,2.35358949949323));
#25529=CARTESIAN_POINT('Ctrl Pts',(5.73012747788933,-1.33590250214437,3.53043767084536));
#25530=CARTESIAN_POINT('Ctrl Pts',(5.58631276176449,1.33590250214434,3.53043767084537));
#25531=CARTESIAN_POINT('Ctrl Pts',(5.49044019744956,2.66764791318187,2.35358949949325));
#25532=CARTESIAN_POINT('Ctrl Pts',(5.44249804563967,3.05727323599639,1.61683334455652));
#25533=CARTESIAN_POINT('Ctrl Pts',(5.73695947687322,-2.84753594834877,1.50591416459154));
#25534=CARTESIAN_POINT('Ctrl Pts',(5.68901732506333,-2.48463998601266,2.19212683660541));
#25535=CARTESIAN_POINT('Ctrl Pts',(5.59314476074839,-1.24425594466219,3.28824001164569));
#25536=CARTESIAN_POINT('Ctrl Pts',(5.44933004462356,1.24425594466217,3.28824001164569));
#25537=CARTESIAN_POINT('Ctrl Pts',(5.35345748030862,2.48463998601265,2.19212683660542));
#25538=CARTESIAN_POINT('Ctrl Pts',(5.30551532849874,2.84753594834877,1.50591416459156));
#25539=CARTESIAN_POINT('Ctrl Pts',(7.39790775678633,-3.47674899880063,1.83866945897147));
#25540=CARTESIAN_POINT('Ctrl Pts',(7.34996556214635,-3.03366513383357,2.67651363411353));
#25541=CARTESIAN_POINT('Ctrl Pts',(7.2540929550013,-1.51914295842827,4.01481425618425));
#25542=CARTESIAN_POINT('Ctrl Pts',(7.11027815321627,1.51914295842826,4.01481425618426));
#25543=CARTESIAN_POINT('Ctrl Pts',(7.01440554607122,3.03366513383357,2.67651363411354));
#25544=CARTESIAN_POINT('Ctrl Pts',(6.96646335143124,3.47674899880063,1.83866945897148));
#25545=CARTESIAN_POINT('Ctrl Pts',(7.26092396320754,-3.26700999135715,1.72774954284456));
#25546=CARTESIAN_POINT('Ctrl Pts',(7.21298176856756,-2.85065568612663,2.51504977427734));
#25547=CARTESIAN_POINT('Ctrl Pts',(7.1171091614225,-1.4274988574663,3.77261582384055));
#25548=CARTESIAN_POINT('Ctrl Pts',(6.97329435963748,1.42749885746629,3.77261582384056));
#25549=CARTESIAN_POINT('Ctrl Pts',(6.87742175249243,2.85065568612662,2.51504977427735));
#25550=CARTESIAN_POINT('Ctrl Pts',(6.82947955785245,3.26700999135715,1.72774954284456));
#25551=CARTESIAN_POINT('Ctrl Pts',(7.12394016962874,-3.05727098391365,1.61682962671764));
#25552=CARTESIAN_POINT('Ctrl Pts',(7.07599797498876,-2.66764623841967,2.35358591444117));
#25553=CARTESIAN_POINT('Ctrl Pts',(6.98012536784371,-1.33585475650433,3.53041739149685));
#25554=CARTESIAN_POINT('Ctrl Pts',(6.83631056605869,1.33585475650433,3.53041739149685));
#25555=CARTESIAN_POINT('Ctrl Pts',(6.74043795891363,2.66764623841968,2.35358591444116));
#25556=CARTESIAN_POINT('Ctrl Pts',(6.69249576427365,3.05727098391365,1.61682962671763));
#25557=CARTESIAN_POINT('Ctrl Pts',(6.98695637604995,-2.84753197647016,1.50590971059071));
#25558=CARTESIAN_POINT('Ctrl Pts',(6.93901418140997,-2.48463679071273,2.19212205460498));
#25559=CARTESIAN_POINT('Ctrl Pts',(6.84314157426491,-1.24421065554235,3.28821895915314));
#25560=CARTESIAN_POINT('Ctrl Pts',(6.69932677247989,1.24421065554236,3.28821895915314));
#25561=CARTESIAN_POINT('Ctrl Pts',(6.60345416533484,2.48463679071275,2.19212205460497));
#25562=CARTESIAN_POINT('Ctrl Pts',(6.55551197069486,2.84753197647017,1.5059097105907));
#25563=CARTESIAN_POINT('Ctrl Pts',(8.64790787376072,-3.47675007987806,1.83866741470954));
#25564=CARTESIAN_POINT('Ctrl Pts',(8.59996564012927,-3.03366637757612,2.67651254993933));
#25565=CARTESIAN_POINT('Ctrl Pts',(8.50409299399277,-1.51909582299121,4.01479640958979));
#25566=CARTESIAN_POINT('Ctrl Pts',(8.3602781142248,1.51909582299119,4.0147964095898));
#25567=CARTESIAN_POINT('Ctrl Pts',(8.2644054680883,3.03366637757611,2.67651254993935));
#25568=CARTESIAN_POINT('Ctrl Pts',(8.21646323445685,3.47675007987805,1.83866741470956));
#25569=CARTESIAN_POINT('Ctrl Pts',(8.5109231002196,-3.26700950677417,1.72774682840093));
#25570=CARTESIAN_POINT('Ctrl Pts',(8.46298086658815,-2.85065554561516,2.51504760041851));
#25571=CARTESIAN_POINT('Ctrl Pts',(8.36710822045164,-1.42745390994202,3.77259732121807));
#25572=CARTESIAN_POINT('Ctrl Pts',(8.22329334068369,1.42745390994201,3.77259732121807));
#25573=CARTESIAN_POINT('Ctrl Pts',(8.12742069454718,2.85065554561515,2.51504760041852));
#25574=CARTESIAN_POINT('Ctrl Pts',(8.07947846091573,3.26700950677417,1.72774682840094));
#25575=CARTESIAN_POINT('Ctrl Pts',(8.37393832667846,-3.05726893367027,1.61682624209231));
#25576=CARTESIAN_POINT('Ctrl Pts',(8.32599609304702,-2.6676447136542,2.35358265089769));
#25577=CARTESIAN_POINT('Ctrl Pts',(8.2301234469105,-1.33581199689285,3.53039823284634));
#25578=CARTESIAN_POINT('Ctrl Pts',(8.08630856714256,1.33581199689285,3.53039823284634));
#25579=CARTESIAN_POINT('Ctrl Pts',(7.99043592100605,2.6676447136542,2.35358265089769));
#25580=CARTESIAN_POINT('Ctrl Pts',(7.9424936873746,3.05726893367027,1.61682624209231));
#25581=CARTESIAN_POINT('Ctrl Pts',(8.23695355313735,-2.84752836056638,1.50590565578368));
#25582=CARTESIAN_POINT('Ctrl Pts',(8.1890113195059,-2.48463388169324,2.19211770137688));
#25583=CARTESIAN_POINT('Ctrl Pts',(8.09313867336938,-1.24417008384366,3.28819914447461));
#25584=CARTESIAN_POINT('Ctrl Pts',(7.94932379360143,1.24417008384367,3.28819914447461));
#25585=CARTESIAN_POINT('Ctrl Pts',(7.85345114746493,2.48463388169325,2.19211770137687));
#25586=CARTESIAN_POINT('Ctrl Pts',(7.80550891383348,2.84752836056639,1.50590565578368));
#25587=CARTESIAN_POINT('Ctrl Pts',(9.89790798080964,-3.47675106922323,1.83866554390586));
#25588=CARTESIAN_POINT('Ctrl Pts',(9.84996571149522,-3.0336675156804,2.67651155795465));
#25589=CARTESIAN_POINT('Ctrl Pts',(9.75409302967573,-1.51905338615236,4.01477938799308));
#25590=CARTESIAN_POINT('Ctrl Pts',(9.61027807854184,1.51905338615236,4.01477938799308));
#25591=CARTESIAN_POINT('Ctrl Pts',(9.51440539672235,3.0336675156804,2.67651155795466));
#25592=CARTESIAN_POINT('Ctrl Pts',(9.46646312740793,3.47675106922323,1.83866554390586));
#25593=CARTESIAN_POINT('Ctrl Pts',(9.76092231045756,-3.26700906330698,1.72774434428311));
#25594=CARTESIAN_POINT('Ctrl Pts',(9.71298004114314,-2.85065541692697,2.5150456111997));
#25595=CARTESIAN_POINT('Ctrl Pts',(9.61710735932365,-1.42741343323025,3.77257974085613));
#25596=CARTESIAN_POINT('Ctrl Pts',(9.47329240818975,1.42741343323025,3.77257974085613));
#25597=CARTESIAN_POINT('Ctrl Pts',(9.37741972637027,2.85065541692698,2.51504561119969));
#25598=CARTESIAN_POINT('Ctrl Pts',(9.32947745705584,3.26700906330699,1.72774434428311));
#25599=CARTESIAN_POINT('Ctrl Pts',(9.62393664010546,-3.05726705739074,1.61682314466038));
#25600=CARTESIAN_POINT('Ctrl Pts',(9.57599437079105,-2.66764331817354,2.35357966444475));
#25601=CARTESIAN_POINT('Ctrl Pts',(9.48012168897155,-1.33577348030816,3.53038009371919));
#25602=CARTESIAN_POINT('Ctrl Pts',(9.33630673783765,1.33577348030817,3.53038009371917));
#25603=CARTESIAN_POINT('Ctrl Pts',(9.24043405601817,2.66764331817355,2.35357966444474));
#25604=CARTESIAN_POINT('Ctrl Pts',(9.19249178670375,3.05726705739074,1.61682314466037));
#25605=CARTESIAN_POINT('Ctrl Pts',(9.48695096975338,-2.84752505147449,1.50590194503763));
#25606=CARTESIAN_POINT('Ctrl Pts',(9.43900870043896,-2.48463121942011,2.1921137176898));
#25607=CARTESIAN_POINT('Ctrl Pts',(9.34313601861947,-1.24413352738605,3.28818044658224));
#25608=CARTESIAN_POINT('Ctrl Pts',(9.19932106748558,1.24413352738608,3.28818044658223));
#25609=CARTESIAN_POINT('Ctrl Pts',(9.10344838566609,2.48463121942012,2.19211371768978));
#25610=CARTESIAN_POINT('Ctrl Pts',(9.05550611635167,2.8475250514745,1.50590194503761));
#25611=CARTESIAN_POINT('Ctrl Pts',(11.1479080792332,-3.47675197885198,1.8386638238398));
#25612=CARTESIAN_POINT('Ctrl Pts',(11.0999657771109,-3.03366856198811,2.67651064606967));
#25613=CARTESIAN_POINT('Ctrl Pts',(11.0040930624836,-1.51901497956362,4.01476313548051));
#25614=CARTESIAN_POINT('Ctrl Pts',(10.860278045734,1.51901497956361,4.01476313548052));
#25615=CARTESIAN_POINT('Ctrl Pts',(10.7644053311067,3.0336685619881,2.67651064606967));
#25616=CARTESIAN_POINT('Ctrl Pts',(10.7164630289844,3.47675197885198,1.83866382383981));
#25617=CARTESIAN_POINT('Ctrl Pts',(11.0109215843298,-3.2670086555702,1.72774206032147));
#25618=CARTESIAN_POINT('Ctrl Pts',(10.9629792822076,-2.85065529851772,2.5150437824221));
#25619=CARTESIAN_POINT('Ctrl Pts',(10.8671065675802,-1.42737679200625,3.77256301095426));
#25620=CARTESIAN_POINT('Ctrl Pts',(10.7232915508306,1.42737679200625,3.77256301095426));
#25621=CARTESIAN_POINT('Ctrl Pts',(10.6274188362032,2.85065529851772,2.5150437824221));
#25622=CARTESIAN_POINT('Ctrl Pts',(10.579476534081,3.2670086555702,1.72774206032147));
#25623=CARTESIAN_POINT('Ctrl Pts',(10.8739350894265,-3.05726533228842,1.61682029680313));
#25624=CARTESIAN_POINT('Ctrl Pts',(10.8259927873042,-2.66764203504732,2.35357691877453));
#25625=CARTESIAN_POINT('Ctrl Pts',(10.7301200726769,-1.33573860444888,3.53036288642801));
#25626=CARTESIAN_POINT('Ctrl Pts',(10.5863050559272,1.33573860444889,3.53036288642801));
#25627=CARTESIAN_POINT('Ctrl Pts',(10.4904323412999,2.66764203504733,2.35357691877453));
#25628=CARTESIAN_POINT('Ctrl Pts',(10.4424900391776,3.05726533228843,1.61682029680313));
#25629=CARTESIAN_POINT('Ctrl Pts',(10.7369485945231,-2.84752200900663,1.5058985332848));
#25630=CARTESIAN_POINT('Ctrl Pts',(10.6890062924008,-2.48462877157693,2.19211005512697));
#25631=CARTESIAN_POINT('Ctrl Pts',(10.5931335777734,-1.24410041689152,3.28816276190175));
#25632=CARTESIAN_POINT('Ctrl Pts',(10.4493185610239,1.24410041689153,3.28816276190174));
#25633=CARTESIAN_POINT('Ctrl Pts',(10.3534458463965,2.48462877157694,2.19211005512695));
#25634=CARTESIAN_POINT('Ctrl Pts',(10.3055035442743,2.84752200900664,1.50589853328477));
#25635=CARTESIAN_POINT('Origin',(11.0238490761438,-0.429849779945933,0.997913274973232));
#25636=CARTESIAN_POINT('Ctrl Pts',(11.1020448718976,-1.95024171098983,-2.73386013557053));
#25637=CARTESIAN_POINT('Ctrl Pts',(11.0712404028977,-2.37355302340116,-2.43188441726037));
#25638=CARTESIAN_POINT('Ctrl Pts',(11.0404359338978,-2.72516811805232,-2.03009223981615));
#25639=CARTESIAN_POINT('Ctrl Pts',(11.0096314648979,-2.96834053891712,-1.57047394666944));
#25640=CARTESIAN_POINT('Ctrl Pts',(11.0759796066463,-1.92402331790621,-2.69710704016389));
#25641=CARTESIAN_POINT('Ctrl Pts',(11.0451751376464,-2.34164377552606,-2.3991909817614));
#25642=CARTESIAN_POINT('Ctrl Pts',(11.0143706686465,-2.68853187520334,-2.00280036310181));
#25643=CARTESIAN_POINT('Ctrl Pts',(10.9835661996466,-2.9284351678973,-1.54936102357415));
#25644=CARTESIAN_POINT('Ctrl Pts',(11.049914341395,-1.8978049248226,-2.66035394475725));
#25645=CARTESIAN_POINT('Ctrl Pts',(11.0191098723951,-2.30973452765096,-2.36649754626242));
#25646=CARTESIAN_POINT('Ctrl Pts',(10.9883054033952,-2.65189563235436,-1.97550848638747));
#25647=CARTESIAN_POINT('Ctrl Pts',(10.9575009343953,-2.88852979687749,-1.52824810047886));
#25648=CARTESIAN_POINT('Ctrl Pts',(11.0238490761438,-1.87158653173898,-2.62360084935061));
#25649=CARTESIAN_POINT('Ctrl Pts',(10.9930446071439,-2.27782527977586,-2.33380411076345));
#25650=CARTESIAN_POINT('Ctrl Pts',(10.962240138144,-2.61525938950538,-1.94821660967313));
#25651=CARTESIAN_POINT('Ctrl Pts',(10.9314356691441,-2.84862442585768,-1.50713517738357));
#25652=CARTESIAN_POINT('Origin',(11.0238490761448,-0.860372781371823,-0.291674745319531));
#25653=CARTESIAN_POINT('Origin',(11.0238490761438,0.,0.));
#25654=CARTESIAN_POINT('',(12.0768490761438,5.,-6.12323399573677E-16));
#25655=CARTESIAN_POINT('Origin',(12.0768490761438,0.,0.));
#25656=CARTESIAN_POINT('',(11.0238490761438,5.,-6.12323399573677E-16));
#25657=CARTESIAN_POINT('',(11.0238490761438,5.,6.12323399573677E-16));
#25658=CARTESIAN_POINT('Origin',(11.0238490761438,0.,0.));
#25659=CARTESIAN_POINT('Origin',(11.0238490761438,0.,0.));
#25660=CARTESIAN_POINT('Origin',(12.0768490761438,0.,0.));
#25661=CARTESIAN_POINT('',(0.,0.,0.));
#25662=CARTESIAN_POINT('Origin',(78.8794814490059,0.,0.));
#25663=CARTESIAN_POINT('',(77.4376255944759,-5.97848259296207E-16,4.88180150972878));
#25664=CARTESIAN_POINT('Origin',(77.4376255944759,0.,0.));
#25665=CARTESIAN_POINT('',(77.7376255944759,-5.97848259296207E-16,4.88180150972878));
#25666=CARTESIAN_POINT('',(78.8794814490059,-5.97848259296207E-16,4.88180150972878));
#25667=CARTESIAN_POINT('Origin',(77.7376255944759,0.,0.));
#25668=CARTESIAN_POINT('Origin',(77.4376255944759,0.,0.));
#25669=CARTESIAN_POINT('',(77.4376255944759,-5.61108855321787E-16,4.58180150972878));
#25670=CARTESIAN_POINT('Origin',(77.4376255944759,0.,0.));
#25671=CARTESIAN_POINT('Origin',(77.7376255944759,0.,0.));
#25672=CARTESIAN_POINT('Origin',(77.7376255944759,-5.61108855321786E-16,
4.58180150972878));
#25673=CARTESIAN_POINT('Origin',(80.0213373035359,0.,0.));
#25674=CARTESIAN_POINT('',(80.3213373035359,-5.61108855321787E-16,4.58180150972878));
#25675=CARTESIAN_POINT('Origin',(80.3213373035359,0.,0.));
#25676=CARTESIAN_POINT('',(80.0213373035359,-5.97848259296207E-16,4.88180150972878));
#25677=CARTESIAN_POINT('Origin',(80.0213373035359,-5.61108855321786E-16,
4.58180150972878));
#25678=CARTESIAN_POINT('Origin',(80.0213373035359,0.,0.));
#25679=CARTESIAN_POINT('Origin',(80.3213373035359,0.,-4.88180150972878));
#25680=CARTESIAN_POINT('',(80.3213373035359,-5.97848259296207E-16,4.88180150972878));
#25681=CARTESIAN_POINT('Origin',(80.3213373035359,0.,0.));
#25682=CARTESIAN_POINT('Origin',(78.8794814490059,0.,0.));
#25683=CARTESIAN_POINT('',(78.8794814490059,-5.97848259296207E-16,4.88180150972878));
#25684=CARTESIAN_POINT('Origin',(66.9212607628943,0.,0.));
#25685=CARTESIAN_POINT('',(76.270750134144,-2.69912154532077E-16,2.204));
#25686=CARTESIAN_POINT('Origin',(76.270750134144,0.,0.));
#25687=CARTESIAN_POINT('',(81.4430005297901,2.69912154532077E-16,2.204));
#25688=CARTESIAN_POINT('',(66.9212607628943,-2.69912154532077E-16,2.204));
#25689=CARTESIAN_POINT('Origin',(81.4430005297901,0.,0.));
#25690=CARTESIAN_POINT('Origin',(76.951201355153,0.,0.));
#25691=CARTESIAN_POINT('',(77.6316525761621,-9.21957102532866E-16,7.52835105742136));
#25692=CARTESIAN_POINT('Origin',(77.6316525761621,0.,0.));
#25693=CARTESIAN_POINT('',(76.270750134144,-7.86576021887409E-16,6.42288064146376));
#25694=CARTESIAN_POINT('',(76.951201355153,-8.54266562210138E-16,6.97561584944256));
#25695=CARTESIAN_POINT('Origin',(76.270750134144,0.,0.));
#25696=CARTESIAN_POINT('Origin',(76.270750134144,0.,-6.42288064146375));
#25697=CARTESIAN_POINT('Origin',(79.0122297603055,0.,0.));
#25698=CARTESIAN_POINT('',(80.392806944449,-9.21957102532866E-16,7.52835105742136));
#25699=CARTESIAN_POINT('Origin',(80.392806944449,0.,0.));
#25700=CARTESIAN_POINT('',(79.0122297603055,-9.21957102532866E-16,7.52835105742136));
#25701=CARTESIAN_POINT('Origin',(80.9179037371196,0.,0.));
#25702=CARTESIAN_POINT('',(81.4430005297901,-7.86763266135053E-16,6.42440960677665));
#25703=CARTESIAN_POINT('',(80.9179037371196,8.5436018433396E-16,6.97638033209901));
#25704=CARTESIAN_POINT('Origin',(81.4430005297901,0.,0.));
#25705=CARTESIAN_POINT('Origin',(81.4430005297901,0.,0.));
#25706=CARTESIAN_POINT('',(0.,0.,0.));
#25707=CARTESIAN_POINT('Ctrl Pts',(82.4430005297901,1.97158113240038,3.97043534620108));
#25708=CARTESIAN_POINT('Ctrl Pts',(87.2430005297901,1.97158113240038,3.97043534620108));
#25709=CARTESIAN_POINT('Ctrl Pts',(82.4430005297901,2.29671111436096,3.77621792657108));
#25710=CARTESIAN_POINT('Ctrl Pts',(87.2430005297901,2.29671111436096,3.77621792657108));
#25711=CARTESIAN_POINT('Ctrl Pts',(82.4430005297901,2.59552275281558,3.54102114079632));
#25712=CARTESIAN_POINT('Ctrl Pts',(87.2430005297901,2.59552275281558,3.54102114079632));
#25713=CARTESIAN_POINT('Ctrl Pts',(82.4430005297901,3.11908576775695,3.00435277140383));
#25714=CARTESIAN_POINT('Ctrl Pts',(87.2430005297901,3.11908576775695,3.00435277140383));
#25715=CARTESIAN_POINT('Ctrl Pts',(82.4430005297901,3.34301024132503,2.70651491388494));
#25716=CARTESIAN_POINT('Ctrl Pts',(87.2430005297901,3.34301024132503,2.70651491388494));
#25717=CARTESIAN_POINT('Ctrl Pts',(82.4430005297901,3.79251211736076,1.90981794028965));
#25718=CARTESIAN_POINT('Ctrl Pts',(87.2430005297901,3.79251211736076,1.90981794028965));
#25719=CARTESIAN_POINT('Ctrl Pts',(82.4430005297901,3.96610878107774,1.3893796287376));
#25720=CARTESIAN_POINT('Ctrl Pts',(87.2430005297901,3.96610878107774,1.3893796287376));
#25721=CARTESIAN_POINT('Ctrl Pts',(82.4430005297901,4.09877879619631,0.327978495265378));
#25722=CARTESIAN_POINT('Ctrl Pts',(87.2430005297901,4.09877879619631,0.327978495265378));
#25723=CARTESIAN_POINT('Ctrl Pts',(82.4430005297901,4.06307606785725,-0.201870082003989));
#25724=CARTESIAN_POINT('Ctrl Pts',(87.2430005297901,4.06307606785725,-0.201870082003989));
#25725=CARTESIAN_POINT('Ctrl Pts',(82.4430005297901,3.79206680758235,-1.20058842967181));
#25726=CARTESIAN_POINT('Ctrl Pts',(87.2430005297901,3.79206680758235,-1.20058842967181));
#25727=CARTESIAN_POINT('Ctrl Pts',(82.4430005297901,3.56572122172907,-1.66148594501202));
#25728=CARTESIAN_POINT('Ctrl Pts',(87.2430005297901,3.56572122172907,-1.66148594501202));
#25729=CARTESIAN_POINT('Ctrl Pts',(82.4430005297901,2.95711124459234,-2.45497912282895));
#25730=CARTESIAN_POINT('Ctrl Pts',(87.2430005297901,2.95711124459234,-2.45497912282895));
#25731=CARTESIAN_POINT('Ctrl Pts',(82.4430005297901,2.58595465431404,-2.78386901588456));
#25732=CARTESIAN_POINT('Ctrl Pts',(87.2430005297901,2.58595465431404,-2.78386901588456));
#25733=CARTESIAN_POINT('Ctrl Pts',(82.4430005297901,2.16151778945147,-3.03095833168073));
#25734=CARTESIAN_POINT('Ctrl Pts',(87.2430005297901,2.16151778945147,-3.03095833168073));
#25735=CARTESIAN_POINT('',(82.4430005297901,1.97158113240038,3.97043534620107));
#25736=CARTESIAN_POINT('',(82.4430005297901,2.16151778945147,-3.03095833168073));
#25737=CARTESIAN_POINT('Ctrl Pts',(82.4430005297901,1.97158113240038,3.97043534620108));
#25738=CARTESIAN_POINT('Ctrl Pts',(82.4430005297901,2.29671111436096,3.77621792657108));
#25739=CARTESIAN_POINT('Ctrl Pts',(82.4430005297901,2.59552275281558,3.54102114079632));
#25740=CARTESIAN_POINT('Ctrl Pts',(82.4430005297901,3.11908576775695,3.00435277140383));
#25741=CARTESIAN_POINT('Ctrl Pts',(82.4430005297901,3.34301024132503,2.70651491388494));
#25742=CARTESIAN_POINT('Ctrl Pts',(82.4430005297901,3.79251211736076,1.90981794028965));
#25743=CARTESIAN_POINT('Ctrl Pts',(82.4430005297901,3.96610878107774,1.3893796287376));
#25744=CARTESIAN_POINT('Ctrl Pts',(82.4430005297901,4.09877879619631,0.327978495265378));
#25745=CARTESIAN_POINT('Ctrl Pts',(82.4430005297901,4.06307606785725,-0.201870082003989));
#25746=CARTESIAN_POINT('Ctrl Pts',(82.4430005297901,3.79206680758235,-1.20058842967181));
#25747=CARTESIAN_POINT('Ctrl Pts',(82.4430005297901,3.56572122172907,-1.66148594501202));
#25748=CARTESIAN_POINT('Ctrl Pts',(82.4430005297901,2.95711124459234,-2.45497912282895));
#25749=CARTESIAN_POINT('Ctrl Pts',(82.4430005297901,2.58595465431404,-2.78386901588456));
#25750=CARTESIAN_POINT('Ctrl Pts',(82.4430005297901,2.16151778945147,-3.03095833168073));
#25751=CARTESIAN_POINT('',(86.4430005297901,2.16151778945147,-3.03095833168073));
#25752=CARTESIAN_POINT('',(82.4430005297901,2.16151778945147,-3.03095833168073));
#25753=CARTESIAN_POINT('',(86.4430005297901,1.97158113240038,3.97043534620107));
#25754=CARTESIAN_POINT('Ctrl Pts',(86.4430005297901,1.97158113240038,3.97043534620108));
#25755=CARTESIAN_POINT('Ctrl Pts',(86.4430005297901,2.29671111436096,3.77621792657108));
#25756=CARTESIAN_POINT('Ctrl Pts',(86.4430005297901,2.59552275281558,3.54102114079632));
#25757=CARTESIAN_POINT('Ctrl Pts',(86.4430005297901,3.11908576775695,3.00435277140383));
#25758=CARTESIAN_POINT('Ctrl Pts',(86.4430005297901,3.34301024132503,2.70651491388494));
#25759=CARTESIAN_POINT('Ctrl Pts',(86.4430005297901,3.79251211736076,1.90981794028965));
#25760=CARTESIAN_POINT('Ctrl Pts',(86.4430005297901,3.96610878107774,1.3893796287376));
#25761=CARTESIAN_POINT('Ctrl Pts',(86.4430005297901,4.09877879619631,0.327978495265378));
#25762=CARTESIAN_POINT('Ctrl Pts',(86.4430005297901,4.06307606785725,-0.201870082003989));
#25763=CARTESIAN_POINT('Ctrl Pts',(86.4430005297901,3.79206680758235,-1.20058842967181));
#25764=CARTESIAN_POINT('Ctrl Pts',(86.4430005297901,3.56572122172907,-1.66148594501202));
#25765=CARTESIAN_POINT('Ctrl Pts',(86.4430005297901,2.95711124459234,-2.45497912282895));
#25766=CARTESIAN_POINT('Ctrl Pts',(86.4430005297901,2.58595465431404,-2.78386901588456));
#25767=CARTESIAN_POINT('Ctrl Pts',(86.4430005297901,2.16151778945147,-3.03095833168073));
#25768=CARTESIAN_POINT('',(82.4430005297901,1.97158113240038,3.97043534620107));
#25769=CARTESIAN_POINT('Origin',(82.4430005297901,-2.77555756156289E-16,
5.55111512312578E-16));
#25770=CARTESIAN_POINT('',(82.4430005297901,-1.97158113240039,3.97043534620107));
#25771=CARTESIAN_POINT('Origin',(82.4430005297901,-2.77555756156289E-16,
5.55111512312578E-16));
#25772=CARTESIAN_POINT('',(86.4430005297901,-1.97158113240039,3.97043534620107));
#25773=CARTESIAN_POINT('Origin',(86.4430005297901,-2.77555756156289E-16,
5.55111512312578E-16));
#25774=CARTESIAN_POINT('',(82.4430005297901,-1.97158113240039,3.97043534620107));
#25775=CARTESIAN_POINT('Ctrl Pts',(82.4430005297901,-2.16151778945139,-3.03095833168078));
#25776=CARTESIAN_POINT('Ctrl Pts',(87.2430005297901,-2.16151778945139,-3.03095833168078));
#25777=CARTESIAN_POINT('Ctrl Pts',(82.4430005297901,-2.4417969811413,-2.86779155838698));
#25778=CARTESIAN_POINT('Ctrl Pts',(87.2430005297901,-2.4417969811413,-2.86779155838698));
#25779=CARTESIAN_POINT('Ctrl Pts',(82.4430005297901,-2.69946597133354,-2.66855779259647));
#25780=CARTESIAN_POINT('Ctrl Pts',(87.2430005297901,-2.69946597133354,-2.66855779259647));
#25781=CARTESIAN_POINT('Ctrl Pts',(82.4430005297901,-3.16313807023027,-2.20413689736136));
#25782=CARTESIAN_POINT('Ctrl Pts',(87.2430005297901,-3.16313807023027,-2.20413689736136));
#25783=CARTESIAN_POINT('Ctrl Pts',(82.4430005297901,-3.36582061002206,-1.93954623621156));
#25784=CARTESIAN_POINT('Ctrl Pts',(87.2430005297901,-3.36582061002206,-1.93954623621156));
#25785=CARTESIAN_POINT('Ctrl Pts',(82.4430005297901,-3.7905877946382,-1.20735040930033));
#25786=CARTESIAN_POINT('Ctrl Pts',(87.2430005297901,-3.7905877946382,-1.20735040930033));
#25787=CARTESIAN_POINT('Ctrl Pts',(82.4430005297901,-3.95787261855977,-0.715467908482556));
#25788=CARTESIAN_POINT('Ctrl Pts',(87.2430005297901,-3.95787261855977,-0.715467908482556));
#25789=CARTESIAN_POINT('Ctrl Pts',(82.4430005297901,-4.0999785741866,0.321696095215354));
#25790=CARTESIAN_POINT('Ctrl Pts',(87.2430005297901,-4.0999785741866,0.321696095215354));
#25791=CARTESIAN_POINT('Ctrl Pts',(82.4430005297901,-4.06691955087291,0.857794436836504));
#25792=CARTESIAN_POINT('Ctrl Pts',(87.2430005297901,-4.06691955087291,0.857794436836504));
#25793=CARTESIAN_POINT('Ctrl Pts',(82.4430005297901,-3.79581350913489,1.90493582172488));
#25794=CARTESIAN_POINT('Ctrl Pts',(87.2430005297901,-3.79581350913489,1.90493582172488));
#25795=CARTESIAN_POINT('Ctrl Pts',(82.4430005297901,-3.55404702294629,2.40416273654669));
#25796=CARTESIAN_POINT('Ctrl Pts',(87.2430005297901,-3.55404702294629,2.40416273654669));
#25797=CARTESIAN_POINT('Ctrl Pts',(82.4430005297901,-2.88474862400959,3.29779955123577));
#25798=CARTESIAN_POINT('Ctrl Pts',(87.2430005297901,-2.88474862400959,3.29779955123577));
#25799=CARTESIAN_POINT('Ctrl Pts',(82.4430005297901,-2.45846445810197,3.67959405679301));
#25800=CARTESIAN_POINT('Ctrl Pts',(87.2430005297901,-2.45846445810197,3.67959405679301));
#25801=CARTESIAN_POINT('Ctrl Pts',(82.4430005297901,-1.97158113240039,3.97043534620107));
#25802=CARTESIAN_POINT('Ctrl Pts',(87.2430005297901,-1.97158113240039,3.97043534620107));
#25803=CARTESIAN_POINT('',(82.4430005297901,-2.16151778945139,-3.03095833168078));
#25804=CARTESIAN_POINT('Ctrl Pts',(82.4430005297901,-2.16151778945139,-3.03095833168078));
#25805=CARTESIAN_POINT('Ctrl Pts',(82.4430005297901,-2.4417969811413,-2.86779155838698));
#25806=CARTESIAN_POINT('Ctrl Pts',(82.4430005297901,-2.69946597133354,-2.66855779259647));
#25807=CARTESIAN_POINT('Ctrl Pts',(82.4430005297901,-3.16313807023027,-2.20413689736136));
#25808=CARTESIAN_POINT('Ctrl Pts',(82.4430005297901,-3.36582061002206,-1.93954623621156));
#25809=CARTESIAN_POINT('Ctrl Pts',(82.4430005297901,-3.7905877946382,-1.20735040930033));
#25810=CARTESIAN_POINT('Ctrl Pts',(82.4430005297901,-3.95787261855977,-0.715467908482556));
#25811=CARTESIAN_POINT('Ctrl Pts',(82.4430005297901,-4.0999785741866,0.321696095215354));
#25812=CARTESIAN_POINT('Ctrl Pts',(82.4430005297901,-4.06691955087291,0.857794436836504));
#25813=CARTESIAN_POINT('Ctrl Pts',(82.4430005297901,-3.79581350913489,1.90493582172488));
#25814=CARTESIAN_POINT('Ctrl Pts',(82.4430005297901,-3.55404702294629,2.40416273654669));
#25815=CARTESIAN_POINT('Ctrl Pts',(82.4430005297901,-2.88474862400959,3.29779955123577));
#25816=CARTESIAN_POINT('Ctrl Pts',(82.4430005297901,-2.45846445810197,3.67959405679301));
#25817=CARTESIAN_POINT('Ctrl Pts',(82.4430005297901,-1.97158113240039,3.97043534620107));
#25818=CARTESIAN_POINT('',(86.4430005297901,-2.16151778945139,-3.03095833168078));
#25819=CARTESIAN_POINT('Ctrl Pts',(86.4430005297901,-2.16151778945139,-3.03095833168078));
#25820=CARTESIAN_POINT('Ctrl Pts',(86.4430005297901,-2.4417969811413,-2.86779155838698));
#25821=CARTESIAN_POINT('Ctrl Pts',(86.4430005297901,-2.69946597133354,-2.66855779259647));
#25822=CARTESIAN_POINT('Ctrl Pts',(86.4430005297901,-3.16313807023027,-2.20413689736136));
#25823=CARTESIAN_POINT('Ctrl Pts',(86.4430005297901,-3.36582061002206,-1.93954623621156));
#25824=CARTESIAN_POINT('Ctrl Pts',(86.4430005297901,-3.7905877946382,-1.20735040930033));
#25825=CARTESIAN_POINT('Ctrl Pts',(86.4430005297901,-3.95787261855977,-0.715467908482556));
#25826=CARTESIAN_POINT('Ctrl Pts',(86.4430005297901,-4.0999785741866,0.321696095215354));
#25827=CARTESIAN_POINT('Ctrl Pts',(86.4430005297901,-4.06691955087291,0.857794436836504));
#25828=CARTESIAN_POINT('Ctrl Pts',(86.4430005297901,-3.79581350913489,1.90493582172488));
#25829=CARTESIAN_POINT('Ctrl Pts',(86.4430005297901,-3.55404702294629,2.40416273654669));
#25830=CARTESIAN_POINT('Ctrl Pts',(86.4430005297901,-2.88474862400959,3.29779955123577));
#25831=CARTESIAN_POINT('Ctrl Pts',(86.4430005297901,-2.45846445810197,3.67959405679301));
#25832=CARTESIAN_POINT('Ctrl Pts',(86.4430005297901,-1.97158113240039,3.97043534620107));
#25833=CARTESIAN_POINT('',(82.4430005297901,-2.16151778945139,-3.03095833168078));
#25834=CARTESIAN_POINT('Origin',(82.4430005297901,-2.77555756156289E-16,
5.55111512312578E-16));
#25835=CARTESIAN_POINT('Origin',(82.4430005297901,-2.77555756156289E-16,
5.55111512312578E-16));
#25836=CARTESIAN_POINT('Origin',(86.4430005297901,-2.77555756156289E-16,
5.55111512312578E-16));
#25837=CARTESIAN_POINT('Origin',(82.4430005297901,7.33246945257534,-3.33066907387547E-15));
#25838=CARTESIAN_POINT('',(82.4430005297901,7.33246945257534,-3.33066907387547E-15));
#25839=CARTESIAN_POINT('',(82.4430005297901,3.66623472628768,6.35010481840362));
#25840=CARTESIAN_POINT('',(82.4430005297901,7.33246945257534,-3.33066907387547E-15));
#25841=CARTESIAN_POINT('',(86.4430005297901,3.66623472628768,6.35010481840362));
#25842=CARTESIAN_POINT('',(82.4430005297901,3.66623472628768,6.35010481840362));
#25843=CARTESIAN_POINT('',(86.4430005297901,7.33246945257534,-3.33066907387547E-15));
#25844=CARTESIAN_POINT('',(86.4430005297901,7.33246945257534,-3.33066907387547E-15));
#25845=CARTESIAN_POINT('',(82.4430005297901,7.33246945257534,-3.33066907387547E-15));
#25846=CARTESIAN_POINT('Origin',(82.4430005297901,3.66623472628767,-6.35010481840363));
#25847=CARTESIAN_POINT('',(82.4430005297901,3.66623472628767,-6.35010481840363));
#25848=CARTESIAN_POINT('',(82.4430005297901,3.66623472628767,-6.35010481840363));
#25849=CARTESIAN_POINT('',(86.4430005297901,3.66623472628767,-6.35010481840363));
#25850=CARTESIAN_POINT('',(86.4430005297901,3.66623472628767,-6.35010481840363));
#25851=CARTESIAN_POINT('',(82.4430005297901,3.66623472628767,-6.35010481840363));
#25852=CARTESIAN_POINT('Origin',(82.4430005297901,-3.66623472628767,-6.35010481840362));
#25853=CARTESIAN_POINT('',(82.4430005297901,-3.66623472628767,-6.35010481840362));
#25854=CARTESIAN_POINT('',(82.4430005297901,-3.66623472628767,-6.35010481840362));
#25855=CARTESIAN_POINT('',(86.4430005297901,-3.66623472628767,-6.35010481840362));
#25856=CARTESIAN_POINT('',(86.4430005297901,-3.66623472628767,-6.35010481840362));
#25857=CARTESIAN_POINT('',(82.4430005297901,-3.66623472628767,-6.35010481840362));
#25858=CARTESIAN_POINT('Origin',(82.4430005297901,-7.33246945257535,2.77555756156289E-15));
#25859=CARTESIAN_POINT('',(82.4430005297901,-7.33246945257535,2.77555756156289E-15));
#25860=CARTESIAN_POINT('',(82.4430005297901,-7.33246945257535,2.77555756156289E-15));
#25861=CARTESIAN_POINT('',(86.4430005297901,-7.33246945257535,2.77555756156289E-15));
#25862=CARTESIAN_POINT('',(86.4430005297901,-7.33246945257535,2.77555756156289E-15));
#25863=CARTESIAN_POINT('',(82.4430005297901,-7.33246945257535,2.77555756156289E-15));
#25864=CARTESIAN_POINT('Origin',(82.4430005297901,-3.66623472628767,6.35010481840363));
#25865=CARTESIAN_POINT('',(82.4430005297901,-3.66623472628767,6.35010481840363));
#25866=CARTESIAN_POINT('',(82.4430005297901,-3.66623472628767,6.35010481840363));
#25867=CARTESIAN_POINT('',(86.4430005297901,-3.66623472628767,6.35010481840363));
#25868=CARTESIAN_POINT('',(86.4430005297901,-3.66623472628767,6.35010481840363));
#25869=CARTESIAN_POINT('',(82.4430005297901,-3.66623472628767,6.35010481840363));
#25870=CARTESIAN_POINT('Origin',(82.4430005297901,3.66623472628768,6.35010481840362));
#25871=CARTESIAN_POINT('',(82.4430005297901,3.66623472628768,6.35010481840362));
#25872=CARTESIAN_POINT('',(86.4430005297901,3.66623472628768,6.35010481840362));
#25873=CARTESIAN_POINT('Origin',(86.4430005297901,0.,0.));
#25874=CARTESIAN_POINT('Origin',(82.4430005297901,0.,0.));
#25875=CARTESIAN_POINT('',(0.,0.,0.));
#25876=CARTESIAN_POINT('Ctrl Pts',(33.9921997677122,5.49976642738082,0.));
#25877=CARTESIAN_POINT('Ctrl Pts',(34.176410294028,5.49976642738082,0.909403588662882));
#25878=CARTESIAN_POINT('Ctrl Pts',(34.5448313466596,5.03991467318512,2.72720954086847));
#25879=CARTESIAN_POINT('Ctrl Pts',(35.0974629256069,3.13419106663809,4.79744756259311));
#25880=CARTESIAN_POINT('Ctrl Pts',(35.6500945045543,0.473252278446431,5.71085179682633));
#25881=CARTESIAN_POINT('Ctrl Pts',(36.2027260835017,-2.30191914515453,5.24783014539696));
#25882=CARTESIAN_POINT('Ctrl Pts',(36.755357662449,-4.52213639346893,3.51971627798693));
#25883=CARTESIAN_POINT('Ctrl Pts',(37.3079892413964,-5.6523152960574,0.943208655172099));
#25884=CARTESIAN_POINT('Ctrl Pts',(37.8606208203438,-5.41997338236277,-1.86068203981508));
#25885=CARTESIAN_POINT('Ctrl Pts',(38.4132523992911,-3.88114100434969,-4.2160410449643));
#25886=CARTESIAN_POINT('Ctrl Pts',(38.9658839782385,-1.40674625429844,-5.55511740772306));
#25887=CARTESIAN_POINT('Ctrl Pts',(39.5185155571859,1.40674646354598,-5.55511666690852));
#25888=CARTESIAN_POINT('Ctrl Pts',(40.0711471361332,3.88114025546219,-4.21604221461142));
#25889=CARTESIAN_POINT('Ctrl Pts',(40.6237787150806,5.41997510425126,-1.86067976428242));
#25890=CARTESIAN_POINT('Ctrl Pts',(41.1764102940279,5.65231160321522,0.943203956408585));
#25891=CARTESIAN_POINT('Ctrl Pts',(41.7290418729754,4.52214418469897,3.51972611893208));
#25892=CARTESIAN_POINT('Ctrl Pts',(42.2816734519227,2.30190265803137,5.24780945677143));
#25893=CARTESIAN_POINT('Ctrl Pts',(42.8343050308701,-0.473218273533045,
5.71089524334113));
#25894=CARTESIAN_POINT('Ctrl Pts',(43.3869366098174,-3.13426874886167,4.79735545609104));
#25895=CARTESIAN_POINT('Ctrl Pts',(43.9395681887648,-5.03979591868312,2.72740116002078));
#25896=CARTESIAN_POINT('Ctrl Pts',(44.4921997677122,-5.73046769283071,-2.96113953592807E-10));
#25897=CARTESIAN_POINT('Ctrl Pts',(45.0448313466595,-5.03979591830015,-2.72740115925713));
#25898=CARTESIAN_POINT('Ctrl Pts',(45.5974629256069,-3.13426874984933,-4.79735545746814));
#25899=CARTESIAN_POINT('Ctrl Pts',(46.1500945045543,-0.473218271369011,
-5.71089524055342));
#25900=CARTESIAN_POINT('Ctrl Pts',(46.7027260835016,2.30190265343826,-5.24780946258346));
#25901=CARTESIAN_POINT('Ctrl Pts',(47.255357662449,4.52214419437993,-3.51972610673135));
#25902=CARTESIAN_POINT('Ctrl Pts',(47.8079892413964,5.65231158284243,-0.943203982060589));
#25903=CARTESIAN_POINT('Ctrl Pts',(48.3606208203438,5.41997514710894,1.86067981823473));
#25904=CARTESIAN_POINT('Ctrl Pts',(48.9132523992911,3.88114016531086,4.21604210112774));
#25905=CARTESIAN_POINT('Ctrl Pts',(49.4658839782385,1.40674665317661,5.55511690561523));
#25906=CARTESIAN_POINT('Ctrl Pts',(50.0185155571858,-1.40674665317677,5.5551169056147));
#25907=CARTESIAN_POINT('Ctrl Pts',(50.5711471361332,-3.8811401653103,4.2160421011286));
#25908=CARTESIAN_POINT('Ctrl Pts',(51.1237787150806,-5.4199751471102,1.86067981823306));
#25909=CARTESIAN_POINT('Ctrl Pts',(51.676410294028,-5.65231158283973,-0.943203982057156));
#25910=CARTESIAN_POINT('Ctrl Pts',(52.2290418729753,-4.52214419438563,-3.51972610673855));
#25911=CARTESIAN_POINT('Ctrl Pts',(52.7816734519227,-2.30190265342625,-5.24780946256834));
#25912=CARTESIAN_POINT('Ctrl Pts',(53.3343050308701,0.473218271343736,-5.71089524058523));
#25913=CARTESIAN_POINT('Ctrl Pts',(53.8869366098175,3.13426874990249,-4.79735545740122));
#25914=CARTESIAN_POINT('Ctrl Pts',(54.4395681887648,5.0397959181883,-2.72740115939791));
#25915=CARTESIAN_POINT('Ctrl Pts',(54.9921997677122,5.73046769306595,-5.11805824213355E-15));
#25916=CARTESIAN_POINT('Ctrl Pts',(55.5448313466596,5.03979591818831,2.72740115939791));
#25917=CARTESIAN_POINT('Ctrl Pts',(56.0974629256069,3.13426874990249,4.79735545740121));
#25918=CARTESIAN_POINT('Ctrl Pts',(56.6500945045543,0.473218271343732,5.71089524058523));
#25919=CARTESIAN_POINT('Ctrl Pts',(57.2027260835016,-2.30190265342626,5.24780946256833));
#25920=CARTESIAN_POINT('Ctrl Pts',(57.755357662449,-4.52214419438564,3.51972610673854));
#25921=CARTESIAN_POINT('Ctrl Pts',(58.3079892413963,-5.65231158283973,0.943203982057152));
#25922=CARTESIAN_POINT('Ctrl Pts',(58.8606208203438,-5.4199751471102,-1.86067981823306));
#25923=CARTESIAN_POINT('Ctrl Pts',(59.4132523992911,-3.88114016531031,-4.2160421011286));
#25924=CARTESIAN_POINT('Ctrl Pts',(59.9658839782385,-1.40674665317677,-5.55511690561469));
#25925=CARTESIAN_POINT('Ctrl Pts',(60.5185155571859,1.40674665317661,-5.55511690561524));
#25926=CARTESIAN_POINT('Ctrl Pts',(61.0711471361332,3.88114016531085,-4.21604210112775));
#25927=CARTESIAN_POINT('Ctrl Pts',(61.6237787150807,5.41997514710894,-1.86067981823474));
#25928=CARTESIAN_POINT('Ctrl Pts',(62.1764102940279,5.65231158284244,0.943203982060585));
#25929=CARTESIAN_POINT('Ctrl Pts',(62.7290418729753,4.52214419437993,3.51972610673135));
#25930=CARTESIAN_POINT('Ctrl Pts',(63.2816734519227,2.30190265343826,5.24780946258346));
#25931=CARTESIAN_POINT('Ctrl Pts',(63.8343050308701,-0.473218271369009,
5.71089524055341));
#25932=CARTESIAN_POINT('Ctrl Pts',(64.3869366098174,-3.13426874984932,4.79735545746814));
#25933=CARTESIAN_POINT('Ctrl Pts',(64.9395681887648,-5.03979591830014,2.72740115925714));
#25934=CARTESIAN_POINT('Ctrl Pts',(65.4921997677122,-5.73046769283071,2.96121409977839E-10));
#25935=CARTESIAN_POINT('Ctrl Pts',(66.0448313466595,-5.03979591868312,-2.72740116002078));
#25936=CARTESIAN_POINT('Ctrl Pts',(66.5974629256069,-3.13426874886167,-4.79735545609105));
#25937=CARTESIAN_POINT('Ctrl Pts',(67.1500945045543,-0.473218273533038,
-5.71089524334112));
#25938=CARTESIAN_POINT('Ctrl Pts',(67.7027260835016,2.30190265803138,-5.24780945677143));
#25939=CARTESIAN_POINT('Ctrl Pts',(68.255357662449,4.52214418469897,-3.51972611893208));
#25940=CARTESIAN_POINT('Ctrl Pts',(68.8079892413964,5.65231160321522,-0.943203956408587));
#25941=CARTESIAN_POINT('Ctrl Pts',(69.3606208203438,5.41997510425126,1.86067976428242));
#25942=CARTESIAN_POINT('Ctrl Pts',(69.9132523992911,3.88114025546219,4.21604221461142));
#25943=CARTESIAN_POINT('Ctrl Pts',(70.4658839782385,1.40674646354597,5.55511666690853));
#25944=CARTESIAN_POINT('Ctrl Pts',(71.0185155571859,-1.40674625429845,5.55511740772306));
#25945=CARTESIAN_POINT('Ctrl Pts',(71.5711471361332,-3.8811410043497,4.21604104496428));
#25946=CARTESIAN_POINT('Ctrl Pts',(72.1237787150806,-5.41997338236277,1.86068203981508));
#25947=CARTESIAN_POINT('Ctrl Pts',(72.676410294028,-5.65231529605741,-0.943208655172103));
#25948=CARTESIAN_POINT('Ctrl Pts',(73.2290418729754,-4.52213639346892,-3.51971627798694));
#25949=CARTESIAN_POINT('Ctrl Pts',(73.7816734519227,-2.30191914515453,-5.24783014539695));
#25950=CARTESIAN_POINT('Ctrl Pts',(74.3343050308701,0.473252278446422,-5.71085179682633));
#25951=CARTESIAN_POINT('Ctrl Pts',(74.8869366098175,3.13419106663809,-4.79744756259312));
#25952=CARTESIAN_POINT('Ctrl Pts',(75.4395681887648,5.03991467318512,-2.72720954086847));
#25953=CARTESIAN_POINT('Ctrl Pts',(75.8079892413964,5.49976642738082,-0.909403588662883));
#25954=CARTESIAN_POINT('Ctrl Pts',(75.9921997677122,5.49976642738082,-8.08232562162E-15));
#25955=CARTESIAN_POINT('Ctrl Pts',(33.9920707665653,5.57474668825,0.));
#25956=CARTESIAN_POINT('Ctrl Pts',(34.1762812928811,5.57474668825,0.921801519276635));
#25957=CARTESIAN_POINT('Ctrl Pts',(34.5447023455127,5.10862550688029,2.76439064201748));
#25958=CARTESIAN_POINT('Ctrl Pts',(35.0973339244601,3.17692056506673,4.86285271511581));
#25959=CARTESIAN_POINT('Ctrl Pts',(35.6499655034074,0.479704279887822,5.78870979651738));
#25960=CARTESIAN_POINT('Ctrl Pts',(36.2025970823548,-2.33330198195422,5.31937556836421));
#25961=CARTESIAN_POINT('Ctrl Pts',(36.7552286613021,-4.5837882052994,3.56770176400508));
#25962=CARTESIAN_POINT('Ctrl Pts',(37.3078602402495,-5.72937521578602,0.956067733435914));
#25963=CARTESIAN_POINT('Ctrl Pts',(37.8604918191969,-5.49386570747434,-1.88604934388851));
#25964=CARTESIAN_POINT('Ctrl Pts',(38.4131233981442,-3.93405390825201,-4.27351975497624));
#25965=CARTESIAN_POINT('Ctrl Pts',(38.9657549770916,-1.42592490042418,-5.63085219620485));
#25966=CARTESIAN_POINT('Ctrl Pts',(39.518386556039,1.42592511248475,-5.63085144582777));
#25967=CARTESIAN_POINT('Ctrl Pts',(40.0710181349864,3.93405314929682,-4.27352093972135));
#25968=CARTESIAN_POINT('Ctrl Pts',(40.6236497139337,5.4938674525111,-1.8860470389829));
#25969=CARTESIAN_POINT('Ctrl Pts',(41.176281292881,5.729371473299,0.95606297402021));
#25970=CARTESIAN_POINT('Ctrl Pts',(41.7289128718285,4.58379610127107,3.56771173198016));
#25971=CARTESIAN_POINT('Ctrl Pts',(42.2815444507758,2.33328527318593,5.31935461269972));
#25972=CARTESIAN_POINT('Ctrl Pts',(42.8341760297232,-0.479669817828385,
5.78875380394745));
#25973=CARTESIAN_POINT('Ctrl Pts',(43.3868076086705,-3.17699929161356,4.8627594207284));
#25974=CARTESIAN_POINT('Ctrl Pts',(43.9394391876179,-5.10850515589866,2.76458473973461));
#25975=CARTESIAN_POINT('Ctrl Pts',(44.4920707665653,-5.80859309124294,-2.99936115018113E-10));
#25976=CARTESIAN_POINT('Ctrl Pts',(45.0447023455126,-5.10850515551054,-2.7645847389611));
#25977=CARTESIAN_POINT('Ctrl Pts',(45.59733392446,-3.17699929261449,-4.86275942212328));
#25978=CARTESIAN_POINT('Ctrl Pts',(46.1499655034074,-0.479669815635259,
-5.78875380112376));
#25979=CARTESIAN_POINT('Ctrl Pts',(46.7025970823548,2.33328526853108,-5.31935461858677));
#25980=CARTESIAN_POINT('Ctrl Pts',(47.2552286613021,4.58379611108217,-3.56771171962194));
#25981=CARTESIAN_POINT('Ctrl Pts',(47.8078602402495,5.72937145265234,-0.956063000003334));
#25982=CARTESIAN_POINT('Ctrl Pts',(48.3604918191969,5.49386749594493,1.88604709363163));
#25983=CARTESIAN_POINT('Ctrl Pts',(48.9131233981442,3.93405305793353,4.27352082477281));
#25984=CARTESIAN_POINT('Ctrl Pts',(49.4657549770916,1.42592530466468,5.63085168761574));
#25985=CARTESIAN_POINT('Ctrl Pts',(50.018386556039,-1.42592530466484,5.6308516876152));
#25986=CARTESIAN_POINT('Ctrl Pts',(50.5710181349864,-3.93405305793297,4.27352082477367));
#25987=CARTESIAN_POINT('Ctrl Pts',(51.1236497139337,-5.49386749594621,1.88604709362994));
#25988=CARTESIAN_POINT('Ctrl Pts',(51.6762812928811,-5.7293714526496,-0.956062999999857));
#25989=CARTESIAN_POINT('Ctrl Pts',(52.2289128718284,-4.58379611108795,-3.56771171962923));
#25990=CARTESIAN_POINT('Ctrl Pts',(52.7815444507759,-2.3332852685189,-5.31935461857145));
#25991=CARTESIAN_POINT('Ctrl Pts',(53.3341760297232,0.479669815609644,-5.78875380115598));
#25992=CARTESIAN_POINT('Ctrl Pts',(53.8868076086706,3.17699929266837,-4.86275942205549));
#25993=CARTESIAN_POINT('Ctrl Pts',(54.4394391876179,5.10850515539719,-2.7645847391037));
#25994=CARTESIAN_POINT('Ctrl Pts',(54.9920707665653,5.80859309148135,-5.41419043299935E-15));
#25995=CARTESIAN_POINT('Ctrl Pts',(55.5447023455127,5.1085051553972,2.7645847391037));
#25996=CARTESIAN_POINT('Ctrl Pts',(56.0973339244601,3.17699929266837,4.86275942205548));
#25997=CARTESIAN_POINT('Ctrl Pts',(56.6499655034074,0.47966981560964,5.78875380115598));
#25998=CARTESIAN_POINT('Ctrl Pts',(57.2025970823548,-2.33328526851891,5.31935461857144));
#25999=CARTESIAN_POINT('Ctrl Pts',(57.7552286613021,-4.58379611108796,3.56771171962922));
#26000=CARTESIAN_POINT('Ctrl Pts',(58.3078602402495,-5.7293714526496,0.956062999999852));
#26001=CARTESIAN_POINT('Ctrl Pts',(58.8604918191969,-5.49386749594621,-1.88604709362995));
#26002=CARTESIAN_POINT('Ctrl Pts',(59.4131233981442,-3.93405305793297,-4.27352082477368));
#26003=CARTESIAN_POINT('Ctrl Pts',(59.9657549770916,-1.42592530466484,-5.63085168761519));
#26004=CARTESIAN_POINT('Ctrl Pts',(60.518386556039,1.42592530466468,-5.63085168761575));
#26005=CARTESIAN_POINT('Ctrl Pts',(61.0710181349863,3.93405305793353,-4.27352082477281));
#26006=CARTESIAN_POINT('Ctrl Pts',(61.6236497139338,5.49386749594494,-1.88604709363164));
#26007=CARTESIAN_POINT('Ctrl Pts',(62.1762812928811,5.72937145265234,0.95606300000333));
#26008=CARTESIAN_POINT('Ctrl Pts',(62.7289128718285,4.58379611108217,3.56771171962194));
#26009=CARTESIAN_POINT('Ctrl Pts',(63.2815444507758,2.33328526853108,5.31935461858677));
#26010=CARTESIAN_POINT('Ctrl Pts',(63.8341760297232,-0.479669815635258,
5.78875380112375));
#26011=CARTESIAN_POINT('Ctrl Pts',(64.3868076086705,-3.17699929261449,4.86275942212328));
#26012=CARTESIAN_POINT('Ctrl Pts',(64.9394391876179,-5.10850515551053,2.76458473896111));
#26013=CARTESIAN_POINT('Ctrl Pts',(65.4920707665653,-5.80859309124295,2.9994369153224E-10));
#26014=CARTESIAN_POINT('Ctrl Pts',(66.0447023455127,-5.10850515589866,-2.76458473973461));
#26015=CARTESIAN_POINT('Ctrl Pts',(66.59733392446,-3.17699929161356,-4.86275942072841));
#26016=CARTESIAN_POINT('Ctrl Pts',(67.1499655034074,-0.479669817828379,
-5.78875380394745));
#26017=CARTESIAN_POINT('Ctrl Pts',(67.7025970823548,2.33328527318594,-5.31935461269972));
#26018=CARTESIAN_POINT('Ctrl Pts',(68.2552286613022,4.58379610127107,-3.56771173198016));
#26019=CARTESIAN_POINT('Ctrl Pts',(68.8078602402495,5.72937147329901,-0.956062974020212));
#26020=CARTESIAN_POINT('Ctrl Pts',(69.3604918191969,5.4938674525111,1.8860470389829));
#26021=CARTESIAN_POINT('Ctrl Pts',(69.9131233981443,3.93405314929682,4.27352093972134));
#26022=CARTESIAN_POINT('Ctrl Pts',(70.4657549770917,1.42592511248473,5.63085144582777));
#26023=CARTESIAN_POINT('Ctrl Pts',(71.018386556039,-1.42592490042419,5.63085219620485));
#26024=CARTESIAN_POINT('Ctrl Pts',(71.5710181349864,-3.93405390825202,4.27351975497623));
#26025=CARTESIAN_POINT('Ctrl Pts',(72.1236497139337,-5.49386570747434,1.88604934388851));
#26026=CARTESIAN_POINT('Ctrl Pts',(72.6762812928811,-5.72937521578603,-0.956067733435918));
#26027=CARTESIAN_POINT('Ctrl Pts',(73.2289128718285,-4.58378820529939,-3.56770176400509));
#26028=CARTESIAN_POINT('Ctrl Pts',(73.7815444507758,-2.33330198195422,-5.31937556836421));
#26029=CARTESIAN_POINT('Ctrl Pts',(74.3341760297232,0.479704279887813,-5.78870979651738));
#26030=CARTESIAN_POINT('Ctrl Pts',(74.8868076086706,3.17692056506672,-4.86285271511582));
#26031=CARTESIAN_POINT('Ctrl Pts',(75.4394391876179,5.10862550688029,-2.76439064201748));
#26032=CARTESIAN_POINT('Ctrl Pts',(75.8078602402495,5.57474668825,-0.921801519276636));
#26033=CARTESIAN_POINT('Ctrl Pts',(75.9920707665653,5.57474668825,-8.19251482538721E-15));
#26034=CARTESIAN_POINT('Ctrl Pts',(33.9431414536155,5.79981109503712,0.));
#26035=CARTESIAN_POINT('Ctrl Pts',(34.1273519799313,5.79981109503712,0.95899747143683));
#26036=CARTESIAN_POINT('Ctrl Pts',(34.4957730325629,5.31486464408031,2.87600085013837));
#26037=CARTESIAN_POINT('Ctrl Pts',(35.0484046115103,3.30517718677737,5.05916675657821));
#26038=CARTESIAN_POINT('Ctrl Pts',(35.6010361904576,0.499070024096898,6.02240821551781));
#26039=CARTESIAN_POINT('Ctrl Pts',(36.153667769405,-2.42749964852484,5.53412340547436));
#26040=CARTESIAN_POINT('Ctrl Pts',(36.7062993483523,-4.76884068918239,3.71173413415615));
#26041=CARTESIAN_POINT('Ctrl Pts',(37.2589309272997,-5.96067611682369,0.994664977192594));
#26042=CARTESIAN_POINT('Ctrl Pts',(37.8115625062471,-5.71565890873659,-1.96219104782992));
#26043=CARTESIAN_POINT('Ctrl Pts',(38.3641940851944,-4.09287582201278,-4.4460463256512));
#26044=CARTESIAN_POINT('Ctrl Pts',(38.9168256641418,-1.48349100436533,-5.85817564103365));
#26045=CARTESIAN_POINT('Ctrl Pts',(39.4694572430892,1.48349122236704,-5.85817489580175));
#26046=CARTESIAN_POINT('Ctrl Pts',(40.0220888220366,4.09287504179451,-4.44604750227257));
#26047=CARTESIAN_POINT('Ctrl Pts',(40.5747204009839,5.71566070266274,-1.96218875872725));
#26048=CARTESIAN_POINT('Ctrl Pts',(41.1273519799312,5.96067226948622,0.994660250423079));
#26049=CARTESIAN_POINT('Ctrl Pts',(41.6799835588787,4.76884880636957,3.71174403388056));
#26050=CARTESIAN_POINT('Ctrl Pts',(42.232615137826,2.42748247163953,5.5341025943587));
#26051=CARTESIAN_POINT('Ctrl Pts',(42.7852467167734,-0.499034596539813,
6.0224519278597));
#26052=CARTESIAN_POINT('Ctrl Pts',(43.3378782957207,-3.30525811894677,5.0590741705265));
#26053=CARTESIAN_POINT('Ctrl Pts',(43.8905098746681,-5.31474092131558,2.87619395462708));
#26054=CARTESIAN_POINT('Ctrl Pts',(44.4431414536155,-6.04309214833711,-2.97879057897562E-10));
#26055=CARTESIAN_POINT('Ctrl Pts',(44.9957730325628,-5.31474092091659,-2.87619395385888));
#26056=CARTESIAN_POINT('Ctrl Pts',(45.5484046115102,-3.30525811997574,-5.05907417191182));
#26057=CARTESIAN_POINT('Ctrl Pts',(46.1010361904576,-0.499034594285245,
-6.02245192505537));
#26058=CARTESIAN_POINT('Ctrl Pts',(46.653667769405,2.42748246685427,-5.53410260020539));
#26059=CARTESIAN_POINT('Ctrl Pts',(47.2062993483523,4.76884881645555,-3.71174402160707));
#26060=CARTESIAN_POINT('Ctrl Pts',(47.7589309272997,5.96067224826112,-0.994660276228043));
#26061=CARTESIAN_POINT('Ctrl Pts',(48.3115625062471,5.71566074731342,1.96218881300126));
#26062=CARTESIAN_POINT('Ctrl Pts',(48.8641940851944,4.09287494787157,4.44604738811221));
#26063=CARTESIAN_POINT('Ctrl Pts',(49.4168256641418,1.48349141993114,5.85817513593182));
#26064=CARTESIAN_POINT('Ctrl Pts',(49.9694572430891,-1.48349141993129,5.85817513593129));
#26065=CARTESIAN_POINT('Ctrl Pts',(50.5220888220366,-4.09287494787099,4.44604738811307));
#26066=CARTESIAN_POINT('Ctrl Pts',(51.0747204009839,-5.71566074731474,1.96218881299959));
#26067=CARTESIAN_POINT('Ctrl Pts',(51.6273519799313,-5.96067224825831,-0.994660276224589));
#26068=CARTESIAN_POINT('Ctrl Pts',(52.1799835588786,-4.76884881646149,-3.71174402161432));
#26069=CARTESIAN_POINT('Ctrl Pts',(52.7326151378261,-2.42748246684175,-5.53410260019018));
#26070=CARTESIAN_POINT('Ctrl Pts',(53.2852467167734,0.499034594258913,-6.02245192508737));
#26071=CARTESIAN_POINT('Ctrl Pts',(53.8378782957208,3.30525812003113,-5.0590741718445));
#26072=CARTESIAN_POINT('Ctrl Pts',(54.3905098746681,5.31474092080006,-2.8761939540005));
#26073=CARTESIAN_POINT('Ctrl Pts',(54.9431414536155,6.0430921485822,-6.36963580352865E-15));
#26074=CARTESIAN_POINT('Ctrl Pts',(55.4957730325629,5.31474092080007,2.8761939540005));
#26075=CARTESIAN_POINT('Ctrl Pts',(56.0484046115103,3.30525812003113,5.05907417184449));
#26076=CARTESIAN_POINT('Ctrl Pts',(56.6010361904576,0.499034594258907,6.02245192508737));
#26077=CARTESIAN_POINT('Ctrl Pts',(57.1536677694049,-2.42748246684176,5.53410260019017));
#26078=CARTESIAN_POINT('Ctrl Pts',(57.7062993483523,-4.7688488164615,3.71174402161431));
#26079=CARTESIAN_POINT('Ctrl Pts',(58.2589309272996,-5.9606722482583,0.994660276224585));
#26080=CARTESIAN_POINT('Ctrl Pts',(58.8115625062471,-5.71566074731474,-1.96218881299959));
#26081=CARTESIAN_POINT('Ctrl Pts',(59.3641940851944,-4.09287494787099,-4.44604738811308));
#26082=CARTESIAN_POINT('Ctrl Pts',(59.9168256641418,-1.4834914199313,-5.85817513593128));
#26083=CARTESIAN_POINT('Ctrl Pts',(60.4694572430892,1.48349141993113,-5.85817513593183));
#26084=CARTESIAN_POINT('Ctrl Pts',(61.0220888220365,4.09287494787156,-4.44604738811222));
#26085=CARTESIAN_POINT('Ctrl Pts',(61.574720400984,5.71566074731343,-1.96218881300128));
#26086=CARTESIAN_POINT('Ctrl Pts',(62.1273519799312,5.96067224826113,0.994660276228038));
#26087=CARTESIAN_POINT('Ctrl Pts',(62.6799835588787,4.76884881645555,3.71174402160707));
#26088=CARTESIAN_POINT('Ctrl Pts',(63.232615137826,2.42748246685427,5.53410260020538));
#26089=CARTESIAN_POINT('Ctrl Pts',(63.7852467167734,-0.499034594285243,
6.02245192505537));
#26090=CARTESIAN_POINT('Ctrl Pts',(64.3378782957207,-3.30525811997573,5.05907417191182));
#26091=CARTESIAN_POINT('Ctrl Pts',(64.8905098746681,-5.31474092091658,2.87619395385889));
#26092=CARTESIAN_POINT('Ctrl Pts',(65.4431414536155,-6.04309214833712,2.97887036704478E-10));
#26093=CARTESIAN_POINT('Ctrl Pts',(65.9957730325628,-5.31474092131558,-2.87619395462708));
#26094=CARTESIAN_POINT('Ctrl Pts',(66.5484046115102,-3.30525811894677,-5.05907417052651));
#26095=CARTESIAN_POINT('Ctrl Pts',(67.1010361904576,-0.499034596539806,
-6.0224519278597));
#26096=CARTESIAN_POINT('Ctrl Pts',(67.653667769405,2.42748247163954,-5.5341025943587));
#26097=CARTESIAN_POINT('Ctrl Pts',(68.2062993483523,4.76884880636957,-3.71174403388056));
#26098=CARTESIAN_POINT('Ctrl Pts',(68.7589309272997,5.96067226948623,-0.994660250423083));
#26099=CARTESIAN_POINT('Ctrl Pts',(69.3115625062471,5.71566070266274,1.96218875872725));
#26100=CARTESIAN_POINT('Ctrl Pts',(69.8641940851944,4.09287504179451,4.44604750227256));
#26101=CARTESIAN_POINT('Ctrl Pts',(70.4168256641419,1.48349122236702,5.85817489580176));
#26102=CARTESIAN_POINT('Ctrl Pts',(70.9694572430892,-1.48349100436534,5.85817564103365));
#26103=CARTESIAN_POINT('Ctrl Pts',(71.5220888220366,-4.09287582201279,4.44604632565119));
#26104=CARTESIAN_POINT('Ctrl Pts',(72.0747204009839,-5.71565890873659,1.96219104782992));
#26105=CARTESIAN_POINT('Ctrl Pts',(72.6273519799313,-5.9606761168237,-0.994664977192599));
#26106=CARTESIAN_POINT('Ctrl Pts',(73.1799835588787,-4.76884068918239,-3.71173413415616));
#26107=CARTESIAN_POINT('Ctrl Pts',(73.732615137826,-2.42749964852484,-5.53412340547436));
#26108=CARTESIAN_POINT('Ctrl Pts',(74.2852467167734,0.499070024096889,-6.02240821551781));
#26109=CARTESIAN_POINT('Ctrl Pts',(74.8378782957208,3.30517718677736,-5.05916675657822));
#26110=CARTESIAN_POINT('Ctrl Pts',(75.3905098746681,5.31486464408031,-2.87600085013837));
#26111=CARTESIAN_POINT('Ctrl Pts',(75.7589309272997,5.79981109503712,-0.958997471436831));
#26112=CARTESIAN_POINT('Ctrl Pts',(75.9431414536155,5.79981109503712,-8.52326411183583E-15));
#26113=CARTESIAN_POINT('Ctrl Pts',(33.62030855087,6.05892730518855,0.));
#26114=CARTESIAN_POINT('Ctrl Pts',(33.8045190771858,6.05892730518855,1.00170122537842));
#26115=CARTESIAN_POINT('Ctrl Pts',(34.1729401298174,5.55226374371841,3.00453419845087));
#26116=CARTESIAN_POINT('Ctrl Pts',(34.7255717087647,3.45282354398353,5.28512205116659));
#26117=CARTESIAN_POINT('Ctrl Pts',(35.2782032877121,0.52135987967838,6.29143885263431));
#26118=CARTESIAN_POINT('Ctrl Pts',(35.8308348666595,-2.53593227701648,5.78132024999939));
#26119=CARTESIAN_POINT('Ctrl Pts',(36.3834664456069,-4.98186108464976,3.87753730806675));
#26120=CARTESIAN_POINT('Ctrl Pts',(36.9360980245542,-6.22693362925883,1.03909408852531));
#26121=CARTESIAN_POINT('Ctrl Pts',(37.4887296035016,-5.97097223597331,-2.04983951271052));
#26122=CARTESIAN_POINT('Ctrl Pts',(38.0413611824489,-4.27570069868504,-4.64464744982032));
#26123=CARTESIAN_POINT('Ctrl Pts',(38.5939927613963,-1.54975720378295,-6.11985471822127));
#26124=CARTESIAN_POINT('Ctrl Pts',(39.1466243403437,1.54975741221459,-6.11985420086809));
#26125=CARTESIAN_POINT('Ctrl Pts',(39.6992559192911,4.27569995271762,-4.64464826665024));
#26126=CARTESIAN_POINT('Ctrl Pts',(40.2518874982384,5.97097395114776,-2.04983792356467));
#26127=CARTESIAN_POINT('Ctrl Pts',(40.8045190771858,6.22692995081589,1.03909080720973));
#26128=CARTESIAN_POINT('Ctrl Pts',(41.3571506561332,4.98186884549998,3.87754418138483));
#26129=CARTESIAN_POINT('Ctrl Pts',(41.9097822350805,2.53591585418045,5.78130580919469));
#26130=CARTESIAN_POINT('Ctrl Pts',(42.4624138140279,-0.521326007358065,
6.29146924994462));
#26131=CARTESIAN_POINT('Ctrl Pts',(43.0150453929753,-3.45290092330605,5.28505830615491));
#26132=CARTESIAN_POINT('Ctrl Pts',(43.5676769719227,-5.55214545226785,3.00467086174248));
#26133=CARTESIAN_POINT('Ctrl Pts',(44.12030855087,-6.31303145085601,-2.06792707167108E-10));
#26134=CARTESIAN_POINT('Ctrl Pts',(44.6729401298174,-5.55214545188636,-3.00467086120918));
#26135=CARTESIAN_POINT('Ctrl Pts',(45.2255717087647,-3.45290092428985,-5.28505830711662));
#26136=CARTESIAN_POINT('Ctrl Pts',(45.7782032877121,-0.521326005202469,
-6.29146924799781));
#26137=CARTESIAN_POINT('Ctrl Pts',(46.3308348666595,2.53591584960525,-5.78130581325357));
#26138=CARTESIAN_POINT('Ctrl Pts',(46.8834664456069,4.98186885514319,-3.87754417286436));
#26139=CARTESIAN_POINT('Ctrl Pts',(47.4360980245542,6.22692993052255,-1.03909082512399));
#26140=CARTESIAN_POINT('Ctrl Pts',(47.9887296035015,5.97097399383832,2.04983796124264));
#26141=CARTESIAN_POINT('Ctrl Pts',(48.541361182449,4.27569986291781,4.64464818739812));
#26142=CARTESIAN_POINT('Ctrl Pts',(49.0939927613963,1.54975760110581,6.11985436757058));
#26143=CARTESIAN_POINT('Ctrl Pts',(49.6466243403437,-1.54975760110596,6.11985436757021));
#26144=CARTESIAN_POINT('Ctrl Pts',(50.199255919291,-4.27569986291726,4.64464818739871));
#26145=CARTESIAN_POINT('Ctrl Pts',(50.7518874982385,-5.97097399383958,2.04983796124148));
#26146=CARTESIAN_POINT('Ctrl Pts',(51.3045190771858,-6.22692993051986,-1.03909082512159));
#26147=CARTESIAN_POINT('Ctrl Pts',(51.8571506561332,-4.98186885514887,-3.87754417286939));
#26148=CARTESIAN_POINT('Ctrl Pts',(52.4097822350806,-2.53591584959328,-5.781305813243));
#26149=CARTESIAN_POINT('Ctrl Pts',(52.9624138140279,0.521326005177292,-6.29146924802002));
#26150=CARTESIAN_POINT('Ctrl Pts',(53.5150453929753,3.45290092434281,-5.28505830706988));
#26151=CARTESIAN_POINT('Ctrl Pts',(54.0676769719227,5.55214545177497,-3.0046708613075));
#26152=CARTESIAN_POINT('Ctrl Pts',(54.62030855087,6.31303145109033,-5.36390383455044E-15));
#26153=CARTESIAN_POINT('Ctrl Pts',(55.1729401298174,5.55214545177497,3.0046708613075));
#26154=CARTESIAN_POINT('Ctrl Pts',(55.7255717087647,3.45290092434281,5.28505830706987));
#26155=CARTESIAN_POINT('Ctrl Pts',(56.2782032877121,0.521326005177289,6.29146924802003));
#26156=CARTESIAN_POINT('Ctrl Pts',(56.8308348666595,-2.5359158495933,5.781305813243));
#26157=CARTESIAN_POINT('Ctrl Pts',(57.3834664456068,-4.98186885514888,3.87754417286939));
#26158=CARTESIAN_POINT('Ctrl Pts',(57.9360980245542,-6.22692993051986,1.03909082512159));
#26159=CARTESIAN_POINT('Ctrl Pts',(58.4887296035016,-5.97097399383958,-2.04983796124148));
#26160=CARTESIAN_POINT('Ctrl Pts',(59.041361182449,-4.27569986291726,-4.64464818739871));
#26161=CARTESIAN_POINT('Ctrl Pts',(59.5939927613963,-1.54975760110596,-6.11985436757021));
#26162=CARTESIAN_POINT('Ctrl Pts',(60.1466243403437,1.5497576011058,-6.11985436757059));
#26163=CARTESIAN_POINT('Ctrl Pts',(60.699255919291,4.2756998629178,-4.64464818739812));
#26164=CARTESIAN_POINT('Ctrl Pts',(61.2518874982385,5.97097399383833,-2.04983796124265));
#26165=CARTESIAN_POINT('Ctrl Pts',(61.8045190771858,6.22692993052255,1.03909082512398));
#26166=CARTESIAN_POINT('Ctrl Pts',(62.3571506561332,4.98186885514319,3.87754417286436));
#26167=CARTESIAN_POINT('Ctrl Pts',(62.9097822350805,2.53591584960525,5.78130581325356));
#26168=CARTESIAN_POINT('Ctrl Pts',(63.4624138140279,-0.521326005202466,
6.2914692479978));
#26169=CARTESIAN_POINT('Ctrl Pts',(64.0150453929752,-3.45290092428985,5.28505830711661));
#26170=CARTESIAN_POINT('Ctrl Pts',(64.5676769719227,-5.55214545188636,3.00467086120919));
#26171=CARTESIAN_POINT('Ctrl Pts',(65.1203085508701,-6.31303145085602,2.06801021218025E-10));
#26172=CARTESIAN_POINT('Ctrl Pts',(65.6729401298174,-5.55214545226785,-3.00467086174248));
#26173=CARTESIAN_POINT('Ctrl Pts',(66.2255717087647,-3.45290092330605,-5.28505830615491));
#26174=CARTESIAN_POINT('Ctrl Pts',(66.7782032877121,-0.521326007358057,
-6.29146924994462));
#26175=CARTESIAN_POINT('Ctrl Pts',(67.3308348666595,2.53591585418046,-5.78130580919469));
#26176=CARTESIAN_POINT('Ctrl Pts',(67.8834664456069,4.98186884549998,-3.87754418138483));
#26177=CARTESIAN_POINT('Ctrl Pts',(68.4360980245542,6.22692995081589,-1.03909080720973));
#26178=CARTESIAN_POINT('Ctrl Pts',(68.9887296035016,5.97097395114776,2.04983792356467));
#26179=CARTESIAN_POINT('Ctrl Pts',(69.541361182449,4.27569995271762,4.64464826665024));
#26180=CARTESIAN_POINT('Ctrl Pts',(70.0939927613963,1.54975741221458,6.1198542008681));
#26181=CARTESIAN_POINT('Ctrl Pts',(70.6466243403438,-1.54975720378297,6.11985471822127));
#26182=CARTESIAN_POINT('Ctrl Pts',(71.199255919291,-4.27570069868505,4.6446474498203));
#26183=CARTESIAN_POINT('Ctrl Pts',(71.7518874982385,-5.9709722359733,2.04983951271053));
#26184=CARTESIAN_POINT('Ctrl Pts',(72.3045190771858,-6.22693362925883,-1.03909408852532));
#26185=CARTESIAN_POINT('Ctrl Pts',(72.8571506561333,-4.98186108464976,-3.87753730806676));
#26186=CARTESIAN_POINT('Ctrl Pts',(73.4097822350805,-2.53593227701648,-5.78132024999937));
#26187=CARTESIAN_POINT('Ctrl Pts',(73.962413814028,0.521359879678368,-6.29143885263431));
#26188=CARTESIAN_POINT('Ctrl Pts',(74.5150453929753,3.45282354398353,-5.2851220511666));
#26189=CARTESIAN_POINT('Ctrl Pts',(75.0676769719227,5.55226374371841,-3.00453419845087));
#26190=CARTESIAN_POINT('Ctrl Pts',(75.4360980245542,6.05892730518855,-1.00170122537842));
#26191=CARTESIAN_POINT('Ctrl Pts',(75.62030855087,6.05892730518855,-8.90405511667878E-15));
#26192=CARTESIAN_POINT('Ctrl Pts',(33.1358237202237,5.94680344913766,0.));
#26193=CARTESIAN_POINT('Ctrl Pts',(33.3200342465395,5.94680344913766,0.983379197578396));
#26194=CARTESIAN_POINT('Ctrl Pts',(33.6884552991711,5.44959421336945,2.94886771297254));
#26195=CARTESIAN_POINT('Ctrl Pts',(34.2410868781184,3.38895443893944,5.18742673184628));
#26196=CARTESIAN_POINT('Ctrl Pts',(34.7937184570658,0.511722382884761,6.17505868653612));
#26197=CARTESIAN_POINT('Ctrl Pts',(35.3463500360132,-2.48903384632581,5.67440885923965));
#26198=CARTESIAN_POINT('Ctrl Pts',(35.8989816149605,-4.88972305399822,3.80581898848347));
#26199=CARTESIAN_POINT('Ctrl Pts',(36.4516131939079,-6.11177024810298,1.01987909450271));
#26200=CARTESIAN_POINT('Ctrl Pts',(37.0042447728553,-5.86054195732468,-2.01192998939814));
#26201=CARTESIAN_POINT('Ctrl Pts',(37.5568763518026,-4.19662395290879,-4.55874653989111));
#26202=CARTESIAN_POINT('Ctrl Pts',(38.10950793075,-1.52109519307483,-6.00667145344936));
#26203=CARTESIAN_POINT('Ctrl Pts',(38.6621395096974,1.5210954270842,-6.00667054754812));
#26204=CARTESIAN_POINT('Ctrl Pts',(39.2147710886447,4.19662311539983,-4.55874797018865));
#26205=CARTESIAN_POINT('Ctrl Pts',(39.7674026675921,5.86054388297712,-2.01192720677863));
#26206=CARTESIAN_POINT('Ctrl Pts',(40.3200342465395,6.11176611825916,1.01987334860882));
#26207=CARTESIAN_POINT('Ctrl Pts',(40.8726658254868,4.88973176722276,3.80583102214387));
#26208=CARTESIAN_POINT('Ctrl Pts',(41.4252974044342,2.4890154081581,5.67438355771667));
#26209=CARTESIAN_POINT('Ctrl Pts',(41.9779289833816,-0.511684353915735,
6.17511179518466));
#26210=CARTESIAN_POINT('Ctrl Pts',(42.5305605623289,-3.38904131388133,5.18731389692575));
#26211=CARTESIAN_POINT('Ctrl Pts',(43.0831921412763,-5.44946140575937,2.9491010349948));
#26212=CARTESIAN_POINT('Ctrl Pts',(43.6358237202237,-6.19627521287463,-3.62104274501345E-10));
#26213=CARTESIAN_POINT('Ctrl Pts',(44.1884552991711,-5.44946140533107,-2.94910103406097));
#26214=CARTESIAN_POINT('Ctrl Pts',(44.7410868781184,-3.38904131498586,-5.18731389860973));
#26215=CARTESIAN_POINT('Ctrl Pts',(45.2937184570658,-0.511684351495615,
-6.17511179177572));
#26216=CARTESIAN_POINT('Ctrl Pts',(45.8463500360132,2.48901540302145,-5.67438356482389));
#26217=CARTESIAN_POINT('Ctrl Pts',(46.3989816149605,4.88973177804935,-3.80583100722426));
#26218=CARTESIAN_POINT('Ctrl Pts',(46.9516131939079,6.11176609547551,-1.01987337997725));
#26219=CARTESIAN_POINT('Ctrl Pts',(47.5042447728553,5.86054393090647,2.01192727275394));
#26220=CARTESIAN_POINT('Ctrl Pts',(48.0568763518026,4.19662301458021,4.55874783141572));
#26221=CARTESIAN_POINT('Ctrl Pts',(48.60950793075,1.52109563915525,6.00667083944942));
#26222=CARTESIAN_POINT('Ctrl Pts',(49.1621395096974,-1.52109563915541,6.00667083944875));
#26223=CARTESIAN_POINT('Ctrl Pts',(49.7147710886447,-4.1966230145796,4.55874783141676));
#26224=CARTESIAN_POINT('Ctrl Pts',(50.2674026675921,-5.86054393090788,2.0119272727519));
#26225=CARTESIAN_POINT('Ctrl Pts',(50.8200342465394,-6.1117660954725,-1.01987337997305));
#26226=CARTESIAN_POINT('Ctrl Pts',(51.3726658254868,-4.88973177805572,-3.80583100723307));
#26227=CARTESIAN_POINT('Ctrl Pts',(51.9252974044342,-2.48901540300802,-5.67438356480538));
#26228=CARTESIAN_POINT('Ctrl Pts',(52.4779289833816,0.511684351467352,-6.17511179181463));
#26229=CARTESIAN_POINT('Ctrl Pts',(53.030560562329,3.38904131504531,-5.18731389852789));
#26230=CARTESIAN_POINT('Ctrl Pts',(53.5831921412763,5.449461405206,-2.94910103423313));
#26231=CARTESIAN_POINT('Ctrl Pts',(54.1358237202237,6.1962752131377,-6.168489409733E-15));
#26232=CARTESIAN_POINT('Ctrl Pts',(54.688455299171,5.44946140520601,2.94910103423312));
#26233=CARTESIAN_POINT('Ctrl Pts',(55.2410868781184,3.38904131504531,5.18731389852788));
#26234=CARTESIAN_POINT('Ctrl Pts',(55.7937184570658,0.511684351467345,6.17511179181463));
#26235=CARTESIAN_POINT('Ctrl Pts',(56.3463500360131,-2.48901540300803,5.67438356480538));
#26236=CARTESIAN_POINT('Ctrl Pts',(56.8989816149606,-4.88973177805573,3.80583100723306));
#26237=CARTESIAN_POINT('Ctrl Pts',(57.4516131939078,-6.1117660954725,1.01987337997304));
#26238=CARTESIAN_POINT('Ctrl Pts',(58.0042447728553,-5.86054393090788,-2.0119272727519));
#26239=CARTESIAN_POINT('Ctrl Pts',(58.5568763518026,-4.1966230145796,-4.55874783141676));
#26240=CARTESIAN_POINT('Ctrl Pts',(59.1095079307501,-1.52109563915542,-6.00667083944875));
#26241=CARTESIAN_POINT('Ctrl Pts',(59.6621395096973,1.52109563915524,-6.00667083944942));
#26242=CARTESIAN_POINT('Ctrl Pts',(60.2147710886447,4.1966230145802,-4.55874783141572));
#26243=CARTESIAN_POINT('Ctrl Pts',(60.7674026675922,5.86054393090647,-2.01192727275395));
#26244=CARTESIAN_POINT('Ctrl Pts',(61.3200342465394,6.11176609547552,1.01987337997724));
#26245=CARTESIAN_POINT('Ctrl Pts',(61.8726658254869,4.88973177804935,3.80583100722426));
#26246=CARTESIAN_POINT('Ctrl Pts',(62.4252974044342,2.48901540302145,5.67438356482389));
#26247=CARTESIAN_POINT('Ctrl Pts',(62.9779289833816,-0.511684351495617,
6.17511179177572));
#26248=CARTESIAN_POINT('Ctrl Pts',(63.5305605623289,-3.38904131498585,5.18731389860973));
#26249=CARTESIAN_POINT('Ctrl Pts',(64.0831921412763,-5.44946140533107,2.94910103406098));
#26250=CARTESIAN_POINT('Ctrl Pts',(64.6358237202237,-6.19627521287463,3.62109504307536E-10));
#26251=CARTESIAN_POINT('Ctrl Pts',(65.188455299171,-5.44946140575937,-2.94910103499479));
#26252=CARTESIAN_POINT('Ctrl Pts',(65.7410868781184,-3.38904131388132,-5.18731389692575));
#26253=CARTESIAN_POINT('Ctrl Pts',(66.2937184570658,-0.511684353915733,
-6.17511179518466));
#26254=CARTESIAN_POINT('Ctrl Pts',(66.8463500360131,2.48901540815811,-5.67438355771667));
#26255=CARTESIAN_POINT('Ctrl Pts',(67.3989816149605,4.88973176722276,-3.80583102214386));
#26256=CARTESIAN_POINT('Ctrl Pts',(67.9516131939078,6.11176611825917,-1.01987334860882));
#26257=CARTESIAN_POINT('Ctrl Pts',(68.5042447728553,5.86054388297712,2.01192720677863));
#26258=CARTESIAN_POINT('Ctrl Pts',(69.0568763518026,4.19662311539983,4.55874797018865));
#26259=CARTESIAN_POINT('Ctrl Pts',(69.60950793075,1.52109542708419,6.00667054754813));
#26260=CARTESIAN_POINT('Ctrl Pts',(70.1621395096974,-1.52109519307484,6.00667145344936));
#26261=CARTESIAN_POINT('Ctrl Pts',(70.7147710886448,-4.19662395290879,4.5587465398911));
#26262=CARTESIAN_POINT('Ctrl Pts',(71.2674026675922,-5.86054195732468,2.01192998939814));
#26263=CARTESIAN_POINT('Ctrl Pts',(71.8200342465394,-6.11177024810298,-1.01987909450272));
#26264=CARTESIAN_POINT('Ctrl Pts',(72.3726658254869,-4.88972305399822,-3.80581898848348));
#26265=CARTESIAN_POINT('Ctrl Pts',(72.9252974044342,-2.48903384632581,-5.67440885923964));
#26266=CARTESIAN_POINT('Ctrl Pts',(73.4779289833816,0.511722382884753,-6.17505868653612));
#26267=CARTESIAN_POINT('Ctrl Pts',(74.0305605623289,3.38895443893944,-5.18742673184629));
#26268=CARTESIAN_POINT('Ctrl Pts',(74.5831921412763,5.44959421336945,-2.94886771297254));
#26269=CARTESIAN_POINT('Ctrl Pts',(74.9516131939079,5.94680344913766,-0.983379197578397));
#26270=CARTESIAN_POINT('Ctrl Pts',(75.1358237202237,5.94680344913766,-8.73928057097385E-15));
#26271=CARTESIAN_POINT('Ctrl Pts',(32.9926516271063,5.64959965017094,0.));
#26272=CARTESIAN_POINT('Ctrl Pts',(33.1768621534221,5.64959965017094,0.934105498328347));
#26273=CARTESIAN_POINT('Ctrl Pts',(33.5452832060536,5.17719316068765,2.80153095913731));
#26274=CARTESIAN_POINT('Ctrl Pts',(34.097914785001,3.21956825042242,4.92810992359527));
#26275=CARTESIAN_POINT('Ctrl Pts',(34.6505463639483,0.486141746602274,5.86641986341936));
#26276=CARTESIAN_POINT('Ctrl Pts',(35.2031779428958,-2.36462122333319,5.39077403004133));
#26277=CARTESIAN_POINT('Ctrl Pts',(35.7558095218431,-4.64531700059631,3.61559300345088));
#26278=CARTESIAN_POINT('Ctrl Pts',(36.3084411007905,-5.80628073241482,0.968900224297807));
#26279=CARTESIAN_POINT('Ctrl Pts',(36.8610726797378,-5.56761023028957,-1.91136547361583));
#26280=CARTESIAN_POINT('Ctrl Pts',(37.4137042586852,-3.98686087342849,-4.33088362081724));
#26281=CARTESIAN_POINT('Ctrl Pts',(37.9663358376326,-1.44506518185627,-5.7064353192738));
#26282=CARTESIAN_POINT('Ctrl Pts',(38.5189674165799,1.445065386745,-5.7064346943363));
#26283=CARTESIAN_POINT('Ctrl Pts',(39.0715989955273,3.98686014014099,-4.33088460750931));
#26284=CARTESIAN_POINT('Ctrl Pts',(39.6242305744747,5.56761191630958,-1.91136355401326));
#26285=CARTESIAN_POINT('Ctrl Pts',(40.1768621534221,5.80627711649786,0.968896260552868));
#26286=CARTESIAN_POINT('Ctrl Pts',(40.7294937323694,4.64532462952802,3.61560130546583));
#26287=CARTESIAN_POINT('Ctrl Pts',(41.2821253113168,2.36460507965162,5.39075658079754));
#26288=CARTESIAN_POINT('Ctrl Pts',(41.8347568902642,-0.486108450041791,
5.86645653965694));
#26289=CARTESIAN_POINT('Ctrl Pts',(42.3873884692115,-3.21964431445548,4.92803248756168));
#26290=CARTESIAN_POINT('Ctrl Pts',(42.9400200481589,-5.17707687994863,2.80169390094401));
#26291=CARTESIAN_POINT('Ctrl Pts',(43.4926516271062,-5.88656213122846,-2.49796196989472E-10));
#26292=CARTESIAN_POINT('Ctrl Pts',(44.0452832060537,-5.17707687957364,-2.80169390029981));
#26293=CARTESIAN_POINT('Ctrl Pts',(44.597914785001,-3.21964431542256,-4.92803248872338));
#26294=CARTESIAN_POINT('Ctrl Pts',(45.1505463639484,-0.486108447922835,
-5.86645653730528));
#26295=CARTESIAN_POINT('Ctrl Pts',(45.7031779428957,2.36460507515419,-5.39075658570046));
#26296=CARTESIAN_POINT('Ctrl Pts',(46.2558095218431,4.64532463900732,-3.61560129517351));
#26297=CARTESIAN_POINT('Ctrl Pts',(46.8084411007904,5.80627709654946,-0.968896282192427));
#26298=CARTESIAN_POINT('Ctrl Pts',(47.3610726797379,5.5676119582745,1.91136359952644));
#26299=CARTESIAN_POINT('Ctrl Pts',(47.9137042586852,3.98686005186758,4.33088451177657));
#26300=CARTESIAN_POINT('Ctrl Pts',(48.4663358376326,1.44506557242546,5.70643489570486));
#26301=CARTESIAN_POINT('Ctrl Pts',(49.0189674165799,-1.4450655724256,5.7064348957044));
#26302=CARTESIAN_POINT('Ctrl Pts',(49.5715989955273,-3.98686005186705,4.3308845117773));
#26303=CARTESIAN_POINT('Ctrl Pts',(50.1242305744747,-5.56761195827573,1.91136359952503));
#26304=CARTESIAN_POINT('Ctrl Pts',(50.6768621534221,-5.80627709654682,-0.968896282189531));
#26305=CARTESIAN_POINT('Ctrl Pts',(51.2294937323694,-4.6453246390129,-3.61560129517959));
#26306=CARTESIAN_POINT('Ctrl Pts',(51.7821253113168,-2.36460507514243,-5.3907565856877));
#26307=CARTESIAN_POINT('Ctrl Pts',(52.3347568902641,0.486108447898087,-5.86645653733213));
#26308=CARTESIAN_POINT('Ctrl Pts',(52.8873884692115,3.21964431547462,-4.92803248866692));
#26309=CARTESIAN_POINT('Ctrl Pts',(53.4400200481589,5.17707687946413,-2.80169390041857));
#26310=CARTESIAN_POINT('Ctrl Pts',(53.9926516271062,5.88656213145879,-3.62063508832155E-15));
#26311=CARTESIAN_POINT('Ctrl Pts',(54.5452832060537,5.17707687946413,2.80169390041857));
#26312=CARTESIAN_POINT('Ctrl Pts',(55.0979147850009,3.21964431547461,4.92803248866692));
#26313=CARTESIAN_POINT('Ctrl Pts',(55.6505463639484,0.486108447898084,5.86645653733212));
#26314=CARTESIAN_POINT('Ctrl Pts',(56.2031779428957,-2.36460507514244,5.3907565856877));
#26315=CARTESIAN_POINT('Ctrl Pts',(56.7558095218431,-4.64532463901291,3.61560129517958));
#26316=CARTESIAN_POINT('Ctrl Pts',(57.3084411007904,-5.80627709654682,0.968896282189525));
#26317=CARTESIAN_POINT('Ctrl Pts',(57.8610726797378,-5.56761195827573,-1.91136359952503));
#26318=CARTESIAN_POINT('Ctrl Pts',(58.4137042586852,-3.98686005186705,-4.3308845117773));
#26319=CARTESIAN_POINT('Ctrl Pts',(58.9663358376325,-1.44506557242561,-5.7064348957044));
#26320=CARTESIAN_POINT('Ctrl Pts',(59.51896741658,1.44506557242545,-5.70643489570486));
#26321=CARTESIAN_POINT('Ctrl Pts',(60.0715989955273,3.98686005186758,-4.33088451177658));
#26322=CARTESIAN_POINT('Ctrl Pts',(60.6242305744747,5.5676119582745,-1.91136359952644));
#26323=CARTESIAN_POINT('Ctrl Pts',(61.176862153422,5.80627709654946,0.968896282192422));
#26324=CARTESIAN_POINT('Ctrl Pts',(61.7294937323694,4.64532463900732,3.61560129517351));
#26325=CARTESIAN_POINT('Ctrl Pts',(62.2821253113167,2.36460507515419,5.39075658570046));
#26326=CARTESIAN_POINT('Ctrl Pts',(62.8347568902642,-0.486108447922834,
5.86645653730528));
#26327=CARTESIAN_POINT('Ctrl Pts',(63.3873884692115,-3.21964431542255,4.92803248872338));
#26328=CARTESIAN_POINT('Ctrl Pts',(63.9400200481589,-5.17707687957363,2.80169390029982));
#26329=CARTESIAN_POINT('Ctrl Pts',(64.4926516271063,-5.88656213122846,2.49803438259616E-10));
#26330=CARTESIAN_POINT('Ctrl Pts',(65.0452832060536,-5.17707687994864,-2.80169390094401));
#26331=CARTESIAN_POINT('Ctrl Pts',(65.597914785001,-3.21964431445548,-4.92803248756169));
#26332=CARTESIAN_POINT('Ctrl Pts',(66.1505463639484,-0.486108450041783,
-5.86645653965694));
#26333=CARTESIAN_POINT('Ctrl Pts',(66.7031779428957,2.36460507965163,-5.39075658079754));
#26334=CARTESIAN_POINT('Ctrl Pts',(67.255809521843,4.64532462952802,-3.61560130546582));
#26335=CARTESIAN_POINT('Ctrl Pts',(67.8084411007905,5.80627711649786,-0.96889626055287));
#26336=CARTESIAN_POINT('Ctrl Pts',(68.3610726797379,5.56761191630958,1.91136355401326));
#26337=CARTESIAN_POINT('Ctrl Pts',(68.9137042586851,3.98686014014099,4.33088460750931));
#26338=CARTESIAN_POINT('Ctrl Pts',(69.4663358376326,1.44506538674499,5.7064346943363));
#26339=CARTESIAN_POINT('Ctrl Pts',(70.0189674165799,-1.44506518185629,5.7064353192738));
#26340=CARTESIAN_POINT('Ctrl Pts',(70.5715989955273,-3.98686087342849,4.33088362081724));
#26341=CARTESIAN_POINT('Ctrl Pts',(71.1242305744747,-5.56761023028957,1.91136547361582));
#26342=CARTESIAN_POINT('Ctrl Pts',(71.6768621534221,-5.80628073241483,-0.968900224297809));
#26343=CARTESIAN_POINT('Ctrl Pts',(72.2294937323694,-4.64531700059631,-3.61559300345089));
#26344=CARTESIAN_POINT('Ctrl Pts',(72.7821253113168,-2.36462122333319,-5.39077403004132));
#26345=CARTESIAN_POINT('Ctrl Pts',(73.3347568902641,0.486141746602262,-5.86641986341937));
#26346=CARTESIAN_POINT('Ctrl Pts',(73.8873884692115,3.21956825042242,-4.92810992359527));
#26347=CARTESIAN_POINT('Ctrl Pts',(74.4400200481589,5.17719316068764,-2.80153095913731));
#26348=CARTESIAN_POINT('Ctrl Pts',(74.8084411007905,5.64959965017094,-0.934105498328348));
#26349=CARTESIAN_POINT('Ctrl Pts',(74.9926516271063,5.64959965017094,-8.30251695365502E-15));
#26350=CARTESIAN_POINT('Ctrl Pts',(32.9926516271063,5.35040034982906,0.));
#26351=CARTESIAN_POINT('Ctrl Pts',(33.1768621534221,5.35040034982906,0.884711999783592));
#26352=CARTESIAN_POINT('Ctrl Pts',(33.5452832060536,4.90303992219514,2.65314027768598));
#26353=CARTESIAN_POINT('Ctrl Pts',(34.097914785001,3.04907159007201,4.66715881783104));
#26354=CARTESIAN_POINT('Ctrl Pts',(34.6505463639483,0.460399720877627,5.55575434845313));
#26355=CARTESIAN_POINT('Ctrl Pts',(35.2031779428958,-2.23940312125801,5.10530860391639));
#26356=CARTESIAN_POINT('Ctrl Pts',(35.7558095218431,-4.39932305117563,3.42412678374845));
#26357=CARTESIAN_POINT('Ctrl Pts',(36.3084411007905,-5.49880832246205,0.917592835722961));
#26358=CARTESIAN_POINT('Ctrl Pts',(36.8610726797378,-5.272776384942,-1.81014920900501));
#26359=CARTESIAN_POINT('Ctrl Pts',(37.4137042586852,-3.77573601188937,-4.10154073270038));
#26360=CARTESIAN_POINT('Ctrl Pts',(37.9663358376326,-1.36854148671349,-5.40425015093622));
#26361=CARTESIAN_POINT('Ctrl Pts',(38.5189674165799,1.36854169117612,-5.40424941809581));
#26362=CARTESIAN_POINT('Ctrl Pts',(39.0715989955273,3.77573528012686,-4.1015418897575));
#26363=CARTESIAN_POINT('Ctrl Pts',(39.6242305744747,5.27277806745566,-1.81014695796662));
#26364=CARTESIAN_POINT('Ctrl Pts',(40.1768621534221,5.49880471406498,0.917588187532836));
#26365=CARTESIAN_POINT('Ctrl Pts',(40.7294937323694,4.39933066424171,3.42413651873231));
#26366=CARTESIAN_POINT('Ctrl Pts',(41.2821253113168,2.23938701114991,5.10528813768847));
#26367=CARTESIAN_POINT('Ctrl Pts',(41.8347568902642,-0.460366493562869,
5.55579732502866));
#26368=CARTESIAN_POINT('Ctrl Pts',(42.3873884692115,-3.04914749591728,4.66706767925751));
#26369=CARTESIAN_POINT('Ctrl Pts',(42.9400200481589,-4.90292388328124,2.65332971861579));
#26370=CARTESIAN_POINT('Ctrl Pts',(43.4926516271062,-5.57483822100387,-2.9292627494233E-10));
#26371=CARTESIAN_POINT('Ctrl Pts',(44.0452832060537,-4.90292388290702,-2.65332971786037));
#26372=CARTESIAN_POINT('Ctrl Pts',(44.597914785001,-3.04914749688235,-4.66706768061979));
#26373=CARTESIAN_POINT('Ctrl Pts',(45.1505463639484,-0.460366491448323,
-5.55579732227095));
#26374=CARTESIAN_POINT('Ctrl Pts',(45.7031779428957,2.23938700666183,-5.10528814343794));
#26375=CARTESIAN_POINT('Ctrl Pts',(46.2558095218431,4.3993306737013,-3.4241365066629));
#26376=CARTESIAN_POINT('Ctrl Pts',(46.8084411007904,5.49880469415807,-0.917588212908723));
#26377=CARTESIAN_POINT('Ctrl Pts',(47.3610726797379,5.2727781093333,1.81014701133818));
#26378=CARTESIAN_POINT('Ctrl Pts',(47.9137042586852,3.77573519203703,4.10154177749537));
#26379=CARTESIAN_POINT('Ctrl Pts',(48.4663358376326,1.36854187647043,5.40424965423309));
#26380=CARTESIAN_POINT('Ctrl Pts',(49.0189674165799,-1.36854187647057,5.40424965423255));
#26381=CARTESIAN_POINT('Ctrl Pts',(49.5715989955273,-3.7757351920365,4.10154177749621));
#26382=CARTESIAN_POINT('Ctrl Pts',(50.1242305744747,-5.27277810933453,1.81014701133654));
#26383=CARTESIAN_POINT('Ctrl Pts',(50.6768621534221,-5.49880469415544,-0.917588212905327));
#26384=CARTESIAN_POINT('Ctrl Pts',(51.2294937323694,-4.39933067370686,-3.42413650667002));
#26385=CARTESIAN_POINT('Ctrl Pts',(51.7821253113168,-2.23938700665009,-5.10528814342298));
#26386=CARTESIAN_POINT('Ctrl Pts',(52.3347568902641,0.460366491423626,-5.55579732230242));
#26387=CARTESIAN_POINT('Ctrl Pts',(52.8873884692115,3.0491474969343,-4.66706768055358));
#26388=CARTESIAN_POINT('Ctrl Pts',(53.4400200481589,4.90292388279774,-2.65332971799963));
#26389=CARTESIAN_POINT('Ctrl Pts',(53.9926516271062,5.57483822123373,-6.57078219732429E-15));
#26390=CARTESIAN_POINT('Ctrl Pts',(54.5452832060537,4.90292388279775,2.65332971799963));
#26391=CARTESIAN_POINT('Ctrl Pts',(55.0979147850009,3.0491474969343,4.66706768055358));
#26392=CARTESIAN_POINT('Ctrl Pts',(55.6505463639484,0.460366491423622,5.55579732230243));
#26393=CARTESIAN_POINT('Ctrl Pts',(56.2031779428957,-2.2393870066501,5.10528814342297));
#26394=CARTESIAN_POINT('Ctrl Pts',(56.7558095218432,-4.39933067370687,3.42413650667002));
#26395=CARTESIAN_POINT('Ctrl Pts',(57.3084411007904,-5.49880469415543,0.917588212905322));
#26396=CARTESIAN_POINT('Ctrl Pts',(57.8610726797378,-5.27277810933453,-1.81014701133654));
#26397=CARTESIAN_POINT('Ctrl Pts',(58.4137042586852,-3.7757351920365,-4.10154177749621));
#26398=CARTESIAN_POINT('Ctrl Pts',(58.9663358376325,-1.36854187647058,-5.40424965423255));
#26399=CARTESIAN_POINT('Ctrl Pts',(59.51896741658,1.36854187647042,-5.40424965423309));
#26400=CARTESIAN_POINT('Ctrl Pts',(60.0715989955273,3.77573519203703,-4.10154177749537));
#26401=CARTESIAN_POINT('Ctrl Pts',(60.6242305744747,5.2727781093333,-1.81014701133819));
#26402=CARTESIAN_POINT('Ctrl Pts',(61.176862153422,5.49880469415808,0.917588212908717));
#26403=CARTESIAN_POINT('Ctrl Pts',(61.7294937323694,4.39933067370129,3.4241365066629));
#26404=CARTESIAN_POINT('Ctrl Pts',(62.2821253113167,2.23938700666183,5.10528814343794));
#26405=CARTESIAN_POINT('Ctrl Pts',(62.8347568902642,-0.460366491448322,
5.55579732227095));
#26406=CARTESIAN_POINT('Ctrl Pts',(63.3873884692115,-3.04914749688234,4.66706768061979));
#26407=CARTESIAN_POINT('Ctrl Pts',(63.9400200481589,-4.90292388290702,2.65332971786038));
#26408=CARTESIAN_POINT('Ctrl Pts',(64.4926516271063,-5.57483822100388,2.92934052602853E-10));
#26409=CARTESIAN_POINT('Ctrl Pts',(65.0452832060536,-4.90292388328124,-2.65332971861579));
#26410=CARTESIAN_POINT('Ctrl Pts',(65.597914785001,-3.04914749591728,-4.66706767925751));
#26411=CARTESIAN_POINT('Ctrl Pts',(66.1505463639483,-0.460366493562863,
-5.55579732502866));
#26412=CARTESIAN_POINT('Ctrl Pts',(66.7031779428957,2.23938701114991,-5.10528813768846));
#26413=CARTESIAN_POINT('Ctrl Pts',(67.2558095218431,4.39933066424171,-3.4241365187323));
#26414=CARTESIAN_POINT('Ctrl Pts',(67.8084411007905,5.49880471406499,-0.917588187532837));
#26415=CARTESIAN_POINT('Ctrl Pts',(68.3610726797379,5.27277806745566,1.81014695796662));
#26416=CARTESIAN_POINT('Ctrl Pts',(68.9137042586851,3.77573528012686,4.1015418897575));
#26417=CARTESIAN_POINT('Ctrl Pts',(69.4663358376326,1.36854169117611,5.40424941809582));
#26418=CARTESIAN_POINT('Ctrl Pts',(70.0189674165799,-1.36854148671351,5.40425015093621));
#26419=CARTESIAN_POINT('Ctrl Pts',(70.5715989955273,-3.77573601188937,4.10154073270038));
#26420=CARTESIAN_POINT('Ctrl Pts',(71.1242305744747,-5.272776384942,1.81014920900501));
#26421=CARTESIAN_POINT('Ctrl Pts',(71.6768621534221,-5.49880832246205,-0.917592835722964));
#26422=CARTESIAN_POINT('Ctrl Pts',(72.2294937323694,-4.39932305117562,-3.42412678374846));
#26423=CARTESIAN_POINT('Ctrl Pts',(72.7821253113168,-2.23940312125801,-5.10530860391638));
#26424=CARTESIAN_POINT('Ctrl Pts',(73.3347568902641,0.460399720877618,-5.55575434845314));
#26425=CARTESIAN_POINT('Ctrl Pts',(73.8873884692115,3.04907159007201,-4.66715881783104));
#26426=CARTESIAN_POINT('Ctrl Pts',(74.4400200481589,4.90303992219514,-2.65314027768598));
#26427=CARTESIAN_POINT('Ctrl Pts',(74.8084411007905,5.35040034982906,-0.884711999783593));
#26428=CARTESIAN_POINT('Ctrl Pts',(74.9926516271063,5.35040034982906,-7.86282079509004E-15));
#26429=CARTESIAN_POINT('Ctrl Pts',(33.1358791011789,5.05215470582044,0.));
#26430=CARTESIAN_POINT('Ctrl Pts',(33.3200896274947,5.05215470582044,0.835439667818526));
#26431=CARTESIAN_POINT('Ctrl Pts',(33.6885106801263,4.62974731329617,2.50523368528442));
#26432=CARTESIAN_POINT('Ctrl Pts',(34.2411422590737,2.87911375329489,4.40702109952745));
#26433=CARTESIAN_POINT('Ctrl Pts',(34.793773838021,0.43473796291613,5.24607120227223));
#26434=CARTESIAN_POINT('Ctrl Pts',(35.3464054169684,-2.11457900308638,4.8207403763615));
#26435=CARTESIAN_POINT('Ctrl Pts',(35.8990369959157,-4.15410404637352,3.23326447896726));
#26436=CARTESIAN_POINT('Ctrl Pts',(36.4516685748631,-5.19230421072891,0.866446616436196));
#26437=CARTESIAN_POINT('Ctrl Pts',(37.0043001538105,-4.9788711625536,-1.70925152427458));
#26438=CARTESIAN_POINT('Ctrl Pts',(37.5569317327579,-3.56527606954637,-3.87292025722597));
#26439=CARTESIAN_POINT('Ctrl Pts',(38.1095633117052,-1.29225881290354,-5.10301667120488));
#26440=CARTESIAN_POINT('Ctrl Pts',(38.6621948906526,1.29225901197644,-5.10301589795954));
#26441=CARTESIAN_POINT('Ctrl Pts',(39.2148264696,3.56527535707347,-3.87292147807751));
#26442=CARTESIAN_POINT('Ctrl Pts',(39.7674580485474,4.97887280071541,-1.70924914912885));
#26443=CARTESIAN_POINT('Ctrl Pts',(40.3200896274947,5.19230069745088,0.8664417119428));
#26444=CARTESIAN_POINT('Ctrl Pts',(40.8727212064421,4.15411145875562,3.23327475046642));
#26445=CARTESIAN_POINT('Ctrl Pts',(41.4253527853894,2.11456331764827,4.82071877979622));
#26446=CARTESIAN_POINT('Ctrl Pts',(41.9779843643368,-0.434705611488933,
5.24611653333821));
#26447=CARTESIAN_POINT('Ctrl Pts',(42.5306159432842,-2.87918765822658,4.40692478140854));
#26448=CARTESIAN_POINT('Ctrl Pts',(43.0832475222315,-4.62963433322232,2.50543281017431));
#26449=CARTESIAN_POINT('Ctrl Pts',(43.6358791011789,-5.26409608723815,-3.09079671340081E-10));
#26450=CARTESIAN_POINT('Ctrl Pts',(44.1885106801263,-4.62963433285796,-2.50543280937723));
#26451=CARTESIAN_POINT('Ctrl Pts',(44.7411422590737,-2.87918765916621,-4.40692478284593));
#26452=CARTESIAN_POINT('Ctrl Pts',(45.293773838021,-0.434705609430123,-5.24611653042846));
#26453=CARTESIAN_POINT('Ctrl Pts',(45.8464054169684,2.1145633132785,-4.82071878586269));
#26454=CARTESIAN_POINT('Ctrl Pts',(46.3990369959157,4.15411146796585,-3.23327473773157));
#26455=CARTESIAN_POINT('Ctrl Pts',(46.9516685748631,5.19230067806873,-0.866441738717781));
#26456=CARTESIAN_POINT('Ctrl Pts',(47.5043001538105,4.97887284148914,1.70924920544305));
#26457=CARTESIAN_POINT('Ctrl Pts',(48.0569317327578,3.56527527130573,3.87292135962583));
#26458=CARTESIAN_POINT('Ctrl Pts',(48.6095633117053,1.2922591923863,5.10301614711619));
#26459=CARTESIAN_POINT('Ctrl Pts',(49.1621948906526,-1.29225919238644,5.10301614711562));
#26460=CARTESIAN_POINT('Ctrl Pts',(49.7148264696,-3.56527527130521,3.87292135962672));
#26461=CARTESIAN_POINT('Ctrl Pts',(50.2674580485474,-4.97887284149034,1.70924920544131));
#26462=CARTESIAN_POINT('Ctrl Pts',(50.8200896274947,-5.19230067806616,-0.866441738714198));
#26463=CARTESIAN_POINT('Ctrl Pts',(51.3727212064421,-4.15411146797128,-3.23327473773908));
#26464=CARTESIAN_POINT('Ctrl Pts',(51.9253527853894,-2.11456331326706,-4.8207187858469));
#26465=CARTESIAN_POINT('Ctrl Pts',(52.4779843643368,0.434705609406076,-5.24611653046166));
#26466=CARTESIAN_POINT('Ctrl Pts',(53.0306159432842,2.87918765921679,-4.40692478277608));
#26467=CARTESIAN_POINT('Ctrl Pts',(53.5832475222316,4.62963433275156,-2.50543280952418));
#26468=CARTESIAN_POINT('Ctrl Pts',(54.1358791011789,5.26409608746195,-1.74326874622889E-15));
#26469=CARTESIAN_POINT('Ctrl Pts',(54.6885106801263,4.62963433275157,2.50543280952417));
#26470=CARTESIAN_POINT('Ctrl Pts',(55.2411422590736,2.87918765921679,4.40692478277608));
#26471=CARTESIAN_POINT('Ctrl Pts',(55.793773838021,0.434705609406073,5.24611653046167));
#26472=CARTESIAN_POINT('Ctrl Pts',(56.3464054169684,-2.11456331326707,4.82071878584689));
#26473=CARTESIAN_POINT('Ctrl Pts',(56.8990369959158,-4.15411146797128,3.23327473773908));
#26474=CARTESIAN_POINT('Ctrl Pts',(57.4516685748631,-5.19230067806616,0.866441738714194));
#26475=CARTESIAN_POINT('Ctrl Pts',(58.0043001538105,-4.97887284149034,-1.70924920544131));
#26476=CARTESIAN_POINT('Ctrl Pts',(58.5569317327579,-3.56527527130521,-3.87292135962672));
#26477=CARTESIAN_POINT('Ctrl Pts',(59.1095633117052,-1.29225919238644,-5.10301614711562));
#26478=CARTESIAN_POINT('Ctrl Pts',(59.6621948906526,1.29225919238629,-5.10301614711619));
#26479=CARTESIAN_POINT('Ctrl Pts',(60.2148264696,3.56527527130572,-3.87292135962584));
#26480=CARTESIAN_POINT('Ctrl Pts',(60.7674580485473,4.97887284148913,-1.70924920544305));
#26481=CARTESIAN_POINT('Ctrl Pts',(61.3200896274947,5.19230067806873,0.866441738717778));
#26482=CARTESIAN_POINT('Ctrl Pts',(61.8727212064421,4.15411146796585,3.23327473773157));
#26483=CARTESIAN_POINT('Ctrl Pts',(62.4253527853894,2.11456331327849,4.82071878586269));
#26484=CARTESIAN_POINT('Ctrl Pts',(62.9779843643369,-0.434705609430122,
5.24611653042845));
#26485=CARTESIAN_POINT('Ctrl Pts',(63.5306159432841,-2.8791876591662,4.40692478284593));
#26486=CARTESIAN_POINT('Ctrl Pts',(64.0832475222316,-4.62963433285796,2.50543280937724));
#26487=CARTESIAN_POINT('Ctrl Pts',(64.6358791011789,-5.26409608723815,3.09085705731855E-10));
#26488=CARTESIAN_POINT('Ctrl Pts',(65.1885106801263,-4.62963433322232,-2.50543281017431));
#26489=CARTESIAN_POINT('Ctrl Pts',(65.7411422590737,-2.87918765822658,-4.40692478140855));
#26490=CARTESIAN_POINT('Ctrl Pts',(66.293773838021,-0.434705611488927,-5.24611653333821));
#26491=CARTESIAN_POINT('Ctrl Pts',(66.8464054169685,2.11456331764827,-4.82071877979622));
#26492=CARTESIAN_POINT('Ctrl Pts',(67.3990369959157,4.15411145875562,-3.23327475046641));
#26493=CARTESIAN_POINT('Ctrl Pts',(67.9516685748631,5.19230069745088,-0.866441711942802));
#26494=CARTESIAN_POINT('Ctrl Pts',(68.5043001538105,4.97887280071541,1.70924914912885));
#26495=CARTESIAN_POINT('Ctrl Pts',(69.0569317327578,3.56527535707346,3.87292147807751));
#26496=CARTESIAN_POINT('Ctrl Pts',(69.6095633117052,1.29225901197643,5.10301589795954));
#26497=CARTESIAN_POINT('Ctrl Pts',(70.1621948906526,-1.29225881290355,5.10301667120488));
#26498=CARTESIAN_POINT('Ctrl Pts',(70.7148264696,-3.56527606954638,3.87292025722596));
#26499=CARTESIAN_POINT('Ctrl Pts',(71.2674580485474,-4.9788711625536,1.70925152427458));
#26500=CARTESIAN_POINT('Ctrl Pts',(71.8200896274948,-5.19230421072891,-0.866446616436202));
#26501=CARTESIAN_POINT('Ctrl Pts',(72.3727212064421,-4.15410404637352,-3.23326447896727));
#26502=CARTESIAN_POINT('Ctrl Pts',(72.9253527853895,-2.11457900308638,-4.82074037636149));
#26503=CARTESIAN_POINT('Ctrl Pts',(73.4779843643368,0.434737962916119,-5.24607120227223));
#26504=CARTESIAN_POINT('Ctrl Pts',(74.0306159432842,2.87911375329489,-4.40702109952745));
#26505=CARTESIAN_POINT('Ctrl Pts',(74.5832475222315,4.62974731329617,-2.50523368528442));
#26506=CARTESIAN_POINT('Ctrl Pts',(74.9516685748631,5.05215470582044,-0.835439667818527));
#26507=CARTESIAN_POINT('Ctrl Pts',(75.1358791011789,5.05215470582044,-7.4245261071363E-15));
#26508=CARTESIAN_POINT('Ctrl Pts',(33.6197755720781,4.94250112032697,0.));
#26509=CARTESIAN_POINT('Ctrl Pts',(33.8039860983939,4.94250112032697,0.817139076837683));
#26510=CARTESIAN_POINT('Ctrl Pts',(34.1724071510254,4.52920068974087,2.45091075495199));
#26511=CARTESIAN_POINT('Ctrl Pts',(34.7250387299729,2.81660319447189,4.31128469373266));
#26512=CARTESIAN_POINT('Ctrl Pts',(35.2776703089202,0.42529402211631,5.13217251323705));
#26513=CARTESIAN_POINT('Ctrl Pts',(35.8303018878676,-2.06865974125642,4.71605075332317));
#26514=CARTESIAN_POINT('Ctrl Pts',(36.3829334668149,-4.06389977762583,3.16305923338873));
#26515=CARTESIAN_POINT('Ctrl Pts',(36.9355650457623,-5.07955447125059,0.847630025952494));
#26516=CARTESIAN_POINT('Ctrl Pts',(37.4881966247097,-4.87075665964084,-1.67213470664358));
#26517=CARTESIAN_POINT('Ctrl Pts',(38.0408282036571,-3.48785707483957,-3.78882139657513));
#26518=CARTESIAN_POINT('Ctrl Pts',(38.5934597826044,-1.26419784346094,-4.9922059811041));
#26519=CARTESIAN_POINT('Ctrl Pts',(39.1460913615518,1.26419801522272,-4.99220553559825));
#26520=CARTESIAN_POINT('Ctrl Pts',(39.6987229404992,3.48785646011191,-3.78882209996813));
#26521=CARTESIAN_POINT('Ctrl Pts',(40.2513545194465,4.87075807306072,-1.67213333819149));
#26522=CARTESIAN_POINT('Ctrl Pts',(40.8039860983939,5.07955143996455,0.847627200316705));
#26523=CARTESIAN_POINT('Ctrl Pts',(41.3566176773413,4.06390617309189,3.16306515207384));
#26524=CARTESIAN_POINT('Ctrl Pts',(41.9092492562886,2.06864620772757,4.71603831708452));
#26525=CARTESIAN_POINT('Ctrl Pts',(42.461880835236,-0.425266109030922,5.13219868216793));
#26526=CARTESIAN_POINT('Ctrl Pts',(43.0145124141834,-2.81666696027288,4.3112297296128));
#26527=CARTESIAN_POINT('Ctrl Pts',(43.5671439931307,-4.52910320957627,2.45102808648086));
#26528=CARTESIAN_POINT('Ctrl Pts',(44.1197755720781,-5.14978781662001,-1.78074231939325E-10));
#26529=CARTESIAN_POINT('Ctrl Pts',(44.6724071510254,-4.5291032092619,-2.45102808602162));
#26530=CARTESIAN_POINT('Ctrl Pts',(45.2250387299728,-2.8166669610836,-4.31122973044095));
#26531=CARTESIAN_POINT('Ctrl Pts',(45.7776703089202,-0.425266107254567,
-5.13219868049148));
#26532=CARTESIAN_POINT('Ctrl Pts',(46.3303018878675,2.06864620395729,-4.71603832057972));
#26533=CARTESIAN_POINT('Ctrl Pts',(46.882933466815,4.06390618103855,-3.16306514473666));
#26534=CARTESIAN_POINT('Ctrl Pts',(47.4355650457623,5.07955142324146,-0.847627215743122));
#26535=CARTESIAN_POINT('Ctrl Pts',(47.9881966247097,4.87075810824064,1.67213337063694));
#26536=CARTESIAN_POINT('Ctrl Pts',(48.540828203657,3.48785638611078,3.78882203172213));
#26537=CARTESIAN_POINT('Ctrl Pts',(49.0934597826044,1.26419817088188,4.99220567914997));
#26538=CARTESIAN_POINT('Ctrl Pts',(49.6460913615518,-1.264198170882,4.99220567914965));
#26539=CARTESIAN_POINT('Ctrl Pts',(50.1987229404991,-3.48785638611033,3.78882203172264));
#26540=CARTESIAN_POINT('Ctrl Pts',(50.7513545194465,-4.87075810824168,1.67213337063594));
#26541=CARTESIAN_POINT('Ctrl Pts',(51.3039860983939,-5.07955142323925,-0.847627215741061));
#26542=CARTESIAN_POINT('Ctrl Pts',(51.8566176773412,-4.06390618104323,-3.16306514474098));
#26543=CARTESIAN_POINT('Ctrl Pts',(52.4092492562886,-2.06864620394743,-4.71603832057063));
#26544=CARTESIAN_POINT('Ctrl Pts',(52.961880835236,0.425266107233821,-5.13219868051061));
#26545=CARTESIAN_POINT('Ctrl Pts',(53.5145124141833,2.81666696112724,-4.31122973040071));
#26546=CARTESIAN_POINT('Ctrl Pts',(54.0671439931307,4.5291032091701,-2.45102808610628));
#26547=CARTESIAN_POINT('Ctrl Pts',(54.6197755720781,5.14978781681311,-5.90029421800548E-15));
#26548=CARTESIAN_POINT('Ctrl Pts',(55.1724071510255,4.52910320917011,2.45102808610628));
#26549=CARTESIAN_POINT('Ctrl Pts',(55.7250387299728,2.81666696112724,4.3112297304007));
#26550=CARTESIAN_POINT('Ctrl Pts',(56.2776703089202,0.425266107233817,5.13219868051062));
#26551=CARTESIAN_POINT('Ctrl Pts',(56.8303018878676,-2.06864620394744,4.71603832057062));
#26552=CARTESIAN_POINT('Ctrl Pts',(57.3829334668149,-4.06390618104323,3.16306514474098));
#26553=CARTESIAN_POINT('Ctrl Pts',(57.9355650457622,-5.07955142323925,0.847627215741054));
#26554=CARTESIAN_POINT('Ctrl Pts',(58.4881966247097,-4.87075810824168,-1.67213337063594));
#26555=CARTESIAN_POINT('Ctrl Pts',(59.0408282036571,-3.48785638611033,-3.78882203172264));
#26556=CARTESIAN_POINT('Ctrl Pts',(59.5934597826044,-1.26419817088201,-4.99220567914965));
#26557=CARTESIAN_POINT('Ctrl Pts',(60.1460913615518,1.26419817088187,-4.99220567914997));
#26558=CARTESIAN_POINT('Ctrl Pts',(60.6987229404992,3.48785638611077,-3.78882203172213));
#26559=CARTESIAN_POINT('Ctrl Pts',(61.2513545194465,4.87075810824064,-1.67213337063695));
#26560=CARTESIAN_POINT('Ctrl Pts',(61.8039860983939,5.07955142324146,0.847627215743118));
#26561=CARTESIAN_POINT('Ctrl Pts',(62.3566176773412,4.06390618103855,3.16306514473665));
#26562=CARTESIAN_POINT('Ctrl Pts',(62.9092492562886,2.06864620395729,4.71603832057972));
#26563=CARTESIAN_POINT('Ctrl Pts',(63.461880835236,-0.425266107254564,5.13219868049148));
#26564=CARTESIAN_POINT('Ctrl Pts',(64.0145124141834,-2.8166669610836,4.31122973044095));
#26565=CARTESIAN_POINT('Ctrl Pts',(64.5671439931307,-4.5291032092619,2.45102808602162));
#26566=CARTESIAN_POINT('Ctrl Pts',(65.1197755720782,-5.14978781662001,1.78081473209479E-10));
#26567=CARTESIAN_POINT('Ctrl Pts',(65.6724071510254,-4.52910320957627,-2.45102808648086));
#26568=CARTESIAN_POINT('Ctrl Pts',(66.2250387299728,-2.81666696027288,-4.3112297296128));
#26569=CARTESIAN_POINT('Ctrl Pts',(66.7776703089202,-0.425266109030917,
-5.13219868216794));
#26570=CARTESIAN_POINT('Ctrl Pts',(67.3303018878675,2.06864620772757,-4.71603831708452));
#26571=CARTESIAN_POINT('Ctrl Pts',(67.8829334668149,4.06390617309189,-3.16306515207384));
#26572=CARTESIAN_POINT('Ctrl Pts',(68.4355650457623,5.07955143996455,-0.847627200316705));
#26573=CARTESIAN_POINT('Ctrl Pts',(68.9881966247097,4.87075807306072,1.67213333819149));
#26574=CARTESIAN_POINT('Ctrl Pts',(69.540828203657,3.48785646011191,3.78882209996812));
#26575=CARTESIAN_POINT('Ctrl Pts',(70.0934597826044,1.26419801522272,4.99220553559826));
#26576=CARTESIAN_POINT('Ctrl Pts',(70.6460913615518,-1.26419784346096,4.99220598110409));
#26577=CARTESIAN_POINT('Ctrl Pts',(71.1987229404992,-3.48785707483957,3.78882139657512));
#26578=CARTESIAN_POINT('Ctrl Pts',(71.7513545194465,-4.87075665964084,1.67213470664358));
#26579=CARTESIAN_POINT('Ctrl Pts',(72.3039860983939,-5.0795544712506,-0.847630025952498));
#26580=CARTESIAN_POINT('Ctrl Pts',(72.8566176773413,-4.06389977762583,-3.16305923338874));
#26581=CARTESIAN_POINT('Ctrl Pts',(73.4092492562886,-2.06865974125642,-4.71605075332316));
#26582=CARTESIAN_POINT('Ctrl Pts',(73.961880835236,0.425294022116303,-5.13217251323706));
#26583=CARTESIAN_POINT('Ctrl Pts',(74.5145124141834,2.81660319447188,-4.31128469373267));
#26584=CARTESIAN_POINT('Ctrl Pts',(75.0671439931307,4.52920068974087,-2.45091075495198));
#26585=CARTESIAN_POINT('Ctrl Pts',(75.4355650457623,4.94250112032697,-0.817139076837684));
#26586=CARTESIAN_POINT('Ctrl Pts',(75.6197755720781,4.94250112032697,-7.26338181214876E-15));
#26587=CARTESIAN_POINT('Ctrl Pts',(33.9441734627902,5.19996900808372,0.));
#26588=CARTESIAN_POINT('Ctrl Pts',(34.128383989106,5.19996900808372,0.859814026526804));
#26589=CARTESIAN_POINT('Ctrl Pts',(34.4968050417376,4.76517797451894,2.57855204094631));
#26590=CARTESIAN_POINT('Ctrl Pts',(35.0494366206849,2.96334119934827,4.53592553639668));
#26591=CARTESIAN_POINT('Ctrl Pts',(35.6020681996323,0.447454012565768,5.39954421798947));
#26592=CARTESIAN_POINT('Ctrl Pts',(36.1546997785797,-2.17643695412734,4.96176002173633));
#26593=CARTESIAN_POINT('Ctrl Pts',(36.707331357527,-4.27562619453865,3.32785024601096));
#26594=CARTESIAN_POINT('Ctrl Pts',(37.2599629364744,-5.34419675899476,0.891792351082074));
#26595=CARTESIAN_POINT('Ctrl Pts',(37.8125945154218,-5.12452030784397,-1.75925261524249));
#26596=CARTESIAN_POINT('Ctrl Pts',(38.3652260943691,-3.66957259079425,-3.98621664555567));
#26597=CARTESIAN_POINT('Ctrl Pts',(38.9178576733165,-1.33006183535942,-5.25229733317933));
#26598=CARTESIAN_POINT('Ctrl Pts',(39.4704892522639,1.33006203085693,-5.25229666444782));
#26599=CARTESIAN_POINT('Ctrl Pts',(40.0231208312112,3.6695718911175,-3.98621770139316));
#26600=CARTESIAN_POINT('Ctrl Pts',(40.5757524101586,5.12452191658404,-1.75925056112342));
#26601=CARTESIAN_POINT('Ctrl Pts',(41.1283839891059,5.34419330881595,0.891788109530082));
#26602=CARTESIAN_POINT('Ctrl Pts',(41.6810155680534,4.27563347379279,3.32785912949593));
#26603=CARTESIAN_POINT('Ctrl Pts',(42.2336471470007,2.17642155040303,4.96174134693238));
#26604=CARTESIAN_POINT('Ctrl Pts',(42.7862787259481,-0.44742224217709,5.39958344300911));
#26605=CARTESIAN_POINT('Ctrl Pts',(43.3389103048954,-2.96341377693166,4.53584245342762));
#26606=CARTESIAN_POINT('Ctrl Pts',(43.8915418838428,-4.76506702359125,2.57872531691644));
#26607=CARTESIAN_POINT('Ctrl Pts',(44.4441734627902,-5.41808896103925,-2.67301766495115E-10));
#26608=CARTESIAN_POINT('Ctrl Pts',(44.9968050417375,-4.76506702323344,-2.5787253162271));
#26609=CARTESIAN_POINT('Ctrl Pts',(45.5494366206849,-2.96341377785441,-4.53584245467072));
#26610=CARTESIAN_POINT('Ctrl Pts',(46.1020681996323,-0.447422240155257,
-5.39958344049266));
#26611=CARTESIAN_POINT('Ctrl Pts',(46.6546997785796,2.17642154611174,-4.96174135217889));
#26612=CARTESIAN_POINT('Ctrl Pts',(47.207331357527,4.27563348283759,-3.32785911848237));
#26613=CARTESIAN_POINT('Ctrl Pts',(47.7599629364744,5.3441932897819,-0.891788132686083));
#26614=CARTESIAN_POINT('Ctrl Pts',(48.3125945154218,5.12452195662546,1.75925060982603));
#26615=CARTESIAN_POINT('Ctrl Pts',(48.8652260943691,3.66957180689017,3.98621759895172));
#26616=CARTESIAN_POINT('Ctrl Pts',(49.4178576733165,1.33006220802659,5.25229687992779));
#26617=CARTESIAN_POINT('Ctrl Pts',(49.9704892522639,-1.33006220802673,5.2522968799273));
#26618=CARTESIAN_POINT('Ctrl Pts',(50.5231208312112,-3.66957180688966,3.9862175989525));
#26619=CARTESIAN_POINT('Ctrl Pts',(51.0757524101586,-5.12452195662665,1.75925060982452));
#26620=CARTESIAN_POINT('Ctrl Pts',(51.628383989106,-5.34419328977938,-0.891788132682984));
#26621=CARTESIAN_POINT('Ctrl Pts',(52.1810155680533,-4.27563348284292,-3.32785911848886));
#26622=CARTESIAN_POINT('Ctrl Pts',(52.7336471470007,-2.17642154610051,-4.96174135216523));
#26623=CARTESIAN_POINT('Ctrl Pts',(53.2862787259481,0.447422240131642,-5.39958344052137));
#26624=CARTESIAN_POINT('Ctrl Pts',(53.8389103048955,2.96341377790408,-4.53584245461031));
#26625=CARTESIAN_POINT('Ctrl Pts',(54.3915418838428,4.76506702312895,-2.57872531635419));
#26626=CARTESIAN_POINT('Ctrl Pts',(54.9441734627902,5.41808896125903,-4.00057827660221E-15));
#26627=CARTESIAN_POINT('Ctrl Pts',(55.4968050417376,4.76506702312896,2.57872531635418));
#26628=CARTESIAN_POINT('Ctrl Pts',(56.0494366206849,2.96341377790408,4.5358424546103));
#26629=CARTESIAN_POINT('Ctrl Pts',(56.6020681996323,0.44742224013164,5.39958344052138));
#26630=CARTESIAN_POINT('Ctrl Pts',(57.1546997785797,-2.17642154610052,4.96174135216522));
#26631=CARTESIAN_POINT('Ctrl Pts',(57.707331357527,-4.27563348284293,3.32785911848886));
#26632=CARTESIAN_POINT('Ctrl Pts',(58.2599629364744,-5.34419328977938,0.89178813268298));
#26633=CARTESIAN_POINT('Ctrl Pts',(58.8125945154218,-5.12452195662665,-1.75925060982453));
#26634=CARTESIAN_POINT('Ctrl Pts',(59.3652260943691,-3.66957180688966,-3.9862175989525));
#26635=CARTESIAN_POINT('Ctrl Pts',(59.9178576733165,-1.33006220802674,-5.2522968799273));
#26636=CARTESIAN_POINT('Ctrl Pts',(60.4704892522639,1.33006220802658,-5.2522968799278));
#26637=CARTESIAN_POINT('Ctrl Pts',(61.0231208312112,3.66957180689017,-3.98621759895173));
#26638=CARTESIAN_POINT('Ctrl Pts',(61.5757524101587,5.12452195662546,-1.75925060982604));
#26639=CARTESIAN_POINT('Ctrl Pts',(62.128383989106,5.3441932897819,0.891788132686079));
#26640=CARTESIAN_POINT('Ctrl Pts',(62.6810155680533,4.27563348283759,3.32785911848237));
#26641=CARTESIAN_POINT('Ctrl Pts',(63.2336471470007,2.17642154611174,4.96174135217889));
#26642=CARTESIAN_POINT('Ctrl Pts',(63.7862787259481,-0.447422240155256,
5.39958344049265));
#26643=CARTESIAN_POINT('Ctrl Pts',(64.3389103048954,-2.96341377785441,4.53584245467072));
#26644=CARTESIAN_POINT('Ctrl Pts',(64.8915418838428,-4.76506702323344,2.57872531622711));
#26645=CARTESIAN_POINT('Ctrl Pts',(65.4441734627902,-5.41808896103925,2.67308784269264E-10));
#26646=CARTESIAN_POINT('Ctrl Pts',(65.9968050417376,-4.76506702359125,-2.57872531691644));
#26647=CARTESIAN_POINT('Ctrl Pts',(66.5494366206849,-2.96341377693166,-4.53584245342762));
#26648=CARTESIAN_POINT('Ctrl Pts',(67.1020681996323,-0.447422242177083,
-5.39958344300911));
#26649=CARTESIAN_POINT('Ctrl Pts',(67.6546997785796,2.17642155040303,-4.96174134693238));
#26650=CARTESIAN_POINT('Ctrl Pts',(68.2073313575271,4.27563347379279,-3.32785912949593));
#26651=CARTESIAN_POINT('Ctrl Pts',(68.7599629364744,5.34419330881595,-0.891788109530083));
#26652=CARTESIAN_POINT('Ctrl Pts',(69.3125945154218,5.12452191658404,1.75925056112342));
#26653=CARTESIAN_POINT('Ctrl Pts',(69.8652260943691,3.6695718911175,3.98621770139316));
#26654=CARTESIAN_POINT('Ctrl Pts',(70.4178576733165,1.33006203085692,5.25229666444782));
#26655=CARTESIAN_POINT('Ctrl Pts',(70.9704892522639,-1.33006183535944,5.25229733317932));
#26656=CARTESIAN_POINT('Ctrl Pts',(71.5231208312112,-3.66957259079425,3.98621664555566));
#26657=CARTESIAN_POINT('Ctrl Pts',(72.0757524101586,-5.12452030784397,1.75925261524249));
#26658=CARTESIAN_POINT('Ctrl Pts',(72.628383989106,-5.34419675899477,-0.891792351082077));
#26659=CARTESIAN_POINT('Ctrl Pts',(73.1810155680534,-4.27562619453864,-3.32785024601098));
#26660=CARTESIAN_POINT('Ctrl Pts',(73.7336471470007,-2.17643695412734,-4.96176002173632));
#26661=CARTESIAN_POINT('Ctrl Pts',(74.2862787259481,0.447454012565758,-5.39954421798947));
#26662=CARTESIAN_POINT('Ctrl Pts',(74.8389103048955,2.96334119934827,-4.53592553639669));
#26663=CARTESIAN_POINT('Ctrl Pts',(75.3915418838428,4.76517797451894,-2.5785520409463));
#26664=CARTESIAN_POINT('Ctrl Pts',(75.7599629364744,5.19996900808372,-0.859814026526805));
#26665=CARTESIAN_POINT('Ctrl Pts',(75.9441734627902,5.19996900808372,-7.6417504816982E-15));
#26666=CARTESIAN_POINT('Ctrl Pts',(33.992328768859,5.42478616651165,0.));
#26667=CARTESIAN_POINT('Ctrl Pts',(34.1765392951748,5.42478616651165,0.897005658049128));
#26668=CARTESIAN_POINT('Ctrl Pts',(34.5449603478064,4.97120383948995,2.69002843971947));
#26669=CARTESIAN_POINT('Ctrl Pts',(35.0975919267537,3.09146156820945,4.73204241007042));
#26670=CARTESIAN_POINT('Ctrl Pts',(35.6502235057011,0.46680027700504,5.63299379713529));
#26671=CARTESIAN_POINT('Ctrl Pts',(36.2028550846485,-2.27053630835485,5.1762847224297));
#26672=CARTESIAN_POINT('Ctrl Pts',(36.7554866635958,-4.46048458163846,3.47173079196878));
#26673=CARTESIAN_POINT('Ctrl Pts',(37.3081182425432,-5.57525537632878,0.930349576908284));
#26674=CARTESIAN_POINT('Ctrl Pts',(37.8607498214906,-5.34608105725119,-1.83531473574165));
#26675=CARTESIAN_POINT('Ctrl Pts',(38.4133814004379,-3.82822810044738,-4.15856233495235));
#26676=CARTESIAN_POINT('Ctrl Pts',(38.9660129793853,-1.3875676081727,-5.47938261924127));
#26677=CARTESIAN_POINT('Ctrl Pts',(39.5186445583327,1.38756781460722,-5.47938188798928));
#26678=CARTESIAN_POINT('Ctrl Pts',(40.07127613728,3.82822736162757,-4.1585634895015));
#26679=CARTESIAN_POINT('Ctrl Pts',(40.6239077162274,5.34608275599143,-1.83531248958194));
#26680=CARTESIAN_POINT('Ctrl Pts',(41.1765392951747,5.57525173313143,0.93034493879696));
#26681=CARTESIAN_POINT('Ctrl Pts',(41.7291708741222,4.46049226812687,3.471740505884));
#26682=CARTESIAN_POINT('Ctrl Pts',(42.2818024530695,2.27052004287681,5.17626430084314));
#26683=CARTESIAN_POINT('Ctrl Pts',(42.8344340320169,-0.466766729237704,
5.6330366827348));
#26684=CARTESIAN_POINT('Ctrl Pts',(43.3870656109642,-3.09153820610978,4.73195149145368));
#26685=CARTESIAN_POINT('Ctrl Pts',(43.9396971899116,-4.97108668146758,2.69021758030695));
#26686=CARTESIAN_POINT('Ctrl Pts',(44.492328768859,-5.65234229441848,-2.92291792167501E-10));
#26687=CARTESIAN_POINT('Ctrl Pts',(45.0449603478063,-4.97108668108975,-2.69021757955316));
#26688=CARTESIAN_POINT('Ctrl Pts',(45.5975919267537,-3.09153820708416,-4.731951492813));
#26689=CARTESIAN_POINT('Ctrl Pts',(46.1502235057011,-0.466766727102762,
-5.63303667998308));
#26690=CARTESIAN_POINT('Ctrl Pts',(46.7028550846484,2.27052003834545,-5.17626430658015));
#26691=CARTESIAN_POINT('Ctrl Pts',(47.2554866635958,4.46049227767768,-3.47174049384076));
#26692=CARTESIAN_POINT('Ctrl Pts',(47.8081182425432,5.57525171303253,-0.930344964117844));
#26693=CARTESIAN_POINT('Ctrl Pts',(48.3607498214906,5.34608279827294,1.83531254283782));
#26694=CARTESIAN_POINT('Ctrl Pts',(48.9133814004379,3.82822727268818,4.15856337748268));
#26695=CARTESIAN_POINT('Ctrl Pts',(49.4660129793853,1.38756800168855,5.47938212361473));
#26696=CARTESIAN_POINT('Ctrl Pts',(50.0186445583327,-1.3875680016887,5.4793821236142));
#26697=CARTESIAN_POINT('Ctrl Pts',(50.57127613728,-3.82822727268764,4.15856337748353));
#26698=CARTESIAN_POINT('Ctrl Pts',(51.1239077162274,-5.34608279827419,1.83531254283617));
#26699=CARTESIAN_POINT('Ctrl Pts',(51.6765392951748,-5.57525171302987,-0.930344964114455));
#26700=CARTESIAN_POINT('Ctrl Pts',(52.2291708741221,-4.46049227768331,-3.47174049384787));
#26701=CARTESIAN_POINT('Ctrl Pts',(52.7818024530695,-2.27052003833359,-5.17626430656522));
#26702=CARTESIAN_POINT('Ctrl Pts',(53.3344340320169,0.466766727077827,-5.63303668001448));
#26703=CARTESIAN_POINT('Ctrl Pts',(53.8870656109643,3.09153820713661,-4.73195149274695));
#26704=CARTESIAN_POINT('Ctrl Pts',(54.4396971899116,4.97108668097941,-2.69021757969212));
#26705=CARTESIAN_POINT('Ctrl Pts',(54.992328768859,5.65234229465055,-4.82192605126774E-15));
#26706=CARTESIAN_POINT('Ctrl Pts',(55.5449603478064,4.97108668097942,2.69021757969212));
#26707=CARTESIAN_POINT('Ctrl Pts',(56.0975919267537,3.09153820713661,4.73195149274694));
#26708=CARTESIAN_POINT('Ctrl Pts',(56.6502235057011,0.466766727077823,5.63303668001448));
#26709=CARTESIAN_POINT('Ctrl Pts',(57.2028550846485,-2.2705200383336,5.17626430656521));
#26710=CARTESIAN_POINT('Ctrl Pts',(57.7554866635958,-4.46049227768332,3.47174049384786));
#26711=CARTESIAN_POINT('Ctrl Pts',(58.3081182425432,-5.57525171302987,0.930344964114451));
#26712=CARTESIAN_POINT('Ctrl Pts',(58.8607498214906,-5.34608279827419,-1.83531254283618));
#26713=CARTESIAN_POINT('Ctrl Pts',(59.4133814004379,-3.82822727268764,-4.15856337748353));
#26714=CARTESIAN_POINT('Ctrl Pts',(59.9660129793853,-1.3875680016887,-5.47938212361419));
#26715=CARTESIAN_POINT('Ctrl Pts',(60.5186445583327,1.38756800168854,-5.47938212361474));
#26716=CARTESIAN_POINT('Ctrl Pts',(61.07127613728,3.82822727268818,-4.15856337748269));
#26717=CARTESIAN_POINT('Ctrl Pts',(61.6239077162275,5.34608279827295,-1.83531254283783));
#26718=CARTESIAN_POINT('Ctrl Pts',(62.1765392951748,5.57525171303254,0.93034496411784));
#26719=CARTESIAN_POINT('Ctrl Pts',(62.7291708741221,4.46049227767768,3.47174049384076));
#26720=CARTESIAN_POINT('Ctrl Pts',(63.2818024530695,2.27052003834545,5.17626430658015));
#26721=CARTESIAN_POINT('Ctrl Pts',(63.8344340320169,-0.466766727102761,
5.63303667998307));
#26722=CARTESIAN_POINT('Ctrl Pts',(64.3870656109642,-3.09153820708416,4.731951492813));
#26723=CARTESIAN_POINT('Ctrl Pts',(64.9396971899116,-4.97108668108975,2.69021757955317));
#26724=CARTESIAN_POINT('Ctrl Pts',(65.492328768859,-5.65234229441848,2.92299128423437E-10));
#26725=CARTESIAN_POINT('Ctrl Pts',(66.0449603478064,-4.97108668146758,-2.69021758030695));
#26726=CARTESIAN_POINT('Ctrl Pts',(66.5975919267537,-3.09153820610978,-4.73195149145368));
#26727=CARTESIAN_POINT('Ctrl Pts',(67.1502235057011,-0.466766729237698,
-5.6330366827348));
#26728=CARTESIAN_POINT('Ctrl Pts',(67.7028550846484,2.27052004287681,-5.17626430084314));
#26729=CARTESIAN_POINT('Ctrl Pts',(68.2554866635959,4.46049226812687,-3.471740505884));
#26730=CARTESIAN_POINT('Ctrl Pts',(68.8081182425432,5.57525173313144,-0.930344938796962));
#26731=CARTESIAN_POINT('Ctrl Pts',(69.3607498214906,5.34608275599143,1.83531248958194));
#26732=CARTESIAN_POINT('Ctrl Pts',(69.9133814004379,3.82822736162757,4.15856348950149));
#26733=CARTESIAN_POINT('Ctrl Pts',(70.4660129793853,1.38756781460721,5.47938188798929));
#26734=CARTESIAN_POINT('Ctrl Pts',(71.0186445583327,-1.38756760817271,5.47938261924127));
#26735=CARTESIAN_POINT('Ctrl Pts',(71.5712761372801,-3.82822810044738,4.15856233495234));
#26736=CARTESIAN_POINT('Ctrl Pts',(72.1239077162274,-5.34608105725119,1.83531473574165));
#26737=CARTESIAN_POINT('Ctrl Pts',(72.6765392951748,-5.57525537632879,-0.930349576908287));
#26738=CARTESIAN_POINT('Ctrl Pts',(73.2291708741222,-4.46048458163846,-3.4717307919688));
#26739=CARTESIAN_POINT('Ctrl Pts',(73.7818024530695,-2.27053630835485,-5.1762847224297));
#26740=CARTESIAN_POINT('Ctrl Pts',(74.3344340320169,0.46680027700503,-5.63299379713529));
#26741=CARTESIAN_POINT('Ctrl Pts',(74.8870656109643,3.09146156820945,-4.73204241007043));
#26742=CARTESIAN_POINT('Ctrl Pts',(75.4396971899116,4.97120383948995,-2.69002843971946));
#26743=CARTESIAN_POINT('Ctrl Pts',(75.8081182425432,5.42478616651165,-0.897005658049129));
#26744=CARTESIAN_POINT('Ctrl Pts',(75.992328768859,5.42478616651165,-7.9721364178528E-15));
#26745=CARTESIAN_POINT('Ctrl Pts',(33.9921997677122,5.49976642738082,0.));
#26746=CARTESIAN_POINT('Ctrl Pts',(34.176410294028,5.49976642738082,0.909403588662882));
#26747=CARTESIAN_POINT('Ctrl Pts',(34.5448313466596,5.03991467318512,2.72720954086847));
#26748=CARTESIAN_POINT('Ctrl Pts',(35.0974629256069,3.13419106663809,4.79744756259311));
#26749=CARTESIAN_POINT('Ctrl Pts',(35.6500945045543,0.473252278446431,5.71085179682633));
#26750=CARTESIAN_POINT('Ctrl Pts',(36.2027260835017,-2.30191914515453,5.24783014539696));
#26751=CARTESIAN_POINT('Ctrl Pts',(36.755357662449,-4.52213639346893,3.51971627798693));
#26752=CARTESIAN_POINT('Ctrl Pts',(37.3079892413964,-5.6523152960574,0.943208655172099));
#26753=CARTESIAN_POINT('Ctrl Pts',(37.8606208203438,-5.41997338236277,-1.86068203981508));
#26754=CARTESIAN_POINT('Ctrl Pts',(38.4132523992911,-3.88114100434969,-4.2160410449643));
#26755=CARTESIAN_POINT('Ctrl Pts',(38.9658839782385,-1.40674625429844,-5.55511740772306));
#26756=CARTESIAN_POINT('Ctrl Pts',(39.5185155571859,1.40674646354598,-5.55511666690852));
#26757=CARTESIAN_POINT('Ctrl Pts',(40.0711471361332,3.88114025546219,-4.21604221461142));
#26758=CARTESIAN_POINT('Ctrl Pts',(40.6237787150806,5.41997510425126,-1.86067976428242));
#26759=CARTESIAN_POINT('Ctrl Pts',(41.1764102940279,5.65231160321522,0.943203956408585));
#26760=CARTESIAN_POINT('Ctrl Pts',(41.7290418729754,4.52214418469897,3.51972611893208));
#26761=CARTESIAN_POINT('Ctrl Pts',(42.2816734519227,2.30190265803137,5.24780945677143));
#26762=CARTESIAN_POINT('Ctrl Pts',(42.8343050308701,-0.473218273533045,
5.71089524334113));
#26763=CARTESIAN_POINT('Ctrl Pts',(43.3869366098174,-3.13426874886167,4.79735545609104));
#26764=CARTESIAN_POINT('Ctrl Pts',(43.9395681887648,-5.03979591868312,2.72740116002078));
#26765=CARTESIAN_POINT('Ctrl Pts',(44.4921997677122,-5.73046769283071,-2.96113953592807E-10));
#26766=CARTESIAN_POINT('Ctrl Pts',(45.0448313466595,-5.03979591830015,-2.72740115925713));
#26767=CARTESIAN_POINT('Ctrl Pts',(45.5974629256069,-3.13426874984933,-4.79735545746814));
#26768=CARTESIAN_POINT('Ctrl Pts',(46.1500945045543,-0.473218271369011,
-5.71089524055342));
#26769=CARTESIAN_POINT('Ctrl Pts',(46.7027260835016,2.30190265343826,-5.24780946258346));
#26770=CARTESIAN_POINT('Ctrl Pts',(47.255357662449,4.52214419437993,-3.51972610673135));
#26771=CARTESIAN_POINT('Ctrl Pts',(47.8079892413964,5.65231158284243,-0.943203982060589));
#26772=CARTESIAN_POINT('Ctrl Pts',(48.3606208203438,5.41997514710894,1.86067981823473));
#26773=CARTESIAN_POINT('Ctrl Pts',(48.9132523992911,3.88114016531086,4.21604210112774));
#26774=CARTESIAN_POINT('Ctrl Pts',(49.4658839782385,1.40674665317661,5.55511690561523));
#26775=CARTESIAN_POINT('Ctrl Pts',(50.0185155571858,-1.40674665317677,5.5551169056147));
#26776=CARTESIAN_POINT('Ctrl Pts',(50.5711471361332,-3.8811401653103,4.2160421011286));
#26777=CARTESIAN_POINT('Ctrl Pts',(51.1237787150806,-5.4199751471102,1.86067981823306));
#26778=CARTESIAN_POINT('Ctrl Pts',(51.676410294028,-5.65231158283973,-0.943203982057156));
#26779=CARTESIAN_POINT('Ctrl Pts',(52.2290418729753,-4.52214419438563,-3.51972610673855));
#26780=CARTESIAN_POINT('Ctrl Pts',(52.7816734519227,-2.30190265342625,-5.24780946256834));
#26781=CARTESIAN_POINT('Ctrl Pts',(53.3343050308701,0.473218271343736,-5.71089524058523));
#26782=CARTESIAN_POINT('Ctrl Pts',(53.8869366098175,3.13426874990249,-4.79735545740122));
#26783=CARTESIAN_POINT('Ctrl Pts',(54.4395681887648,5.0397959181883,-2.72740115939791));
#26784=CARTESIAN_POINT('Ctrl Pts',(54.9921997677122,5.73046769306595,-5.11805824213355E-15));
#26785=CARTESIAN_POINT('Ctrl Pts',(55.5448313466596,5.03979591818831,2.72740115939791));
#26786=CARTESIAN_POINT('Ctrl Pts',(56.0974629256069,3.13426874990249,4.79735545740121));
#26787=CARTESIAN_POINT('Ctrl Pts',(56.6500945045543,0.473218271343732,5.71089524058523));
#26788=CARTESIAN_POINT('Ctrl Pts',(57.2027260835016,-2.30190265342626,5.24780946256833));
#26789=CARTESIAN_POINT('Ctrl Pts',(57.755357662449,-4.52214419438564,3.51972610673854));
#26790=CARTESIAN_POINT('Ctrl Pts',(58.3079892413963,-5.65231158283973,0.943203982057152));
#26791=CARTESIAN_POINT('Ctrl Pts',(58.8606208203438,-5.4199751471102,-1.86067981823306));
#26792=CARTESIAN_POINT('Ctrl Pts',(59.4132523992911,-3.88114016531031,-4.2160421011286));
#26793=CARTESIAN_POINT('Ctrl Pts',(59.9658839782385,-1.40674665317677,-5.55511690561469));
#26794=CARTESIAN_POINT('Ctrl Pts',(60.5185155571859,1.40674665317661,-5.55511690561524));
#26795=CARTESIAN_POINT('Ctrl Pts',(61.0711471361332,3.88114016531085,-4.21604210112775));
#26796=CARTESIAN_POINT('Ctrl Pts',(61.6237787150807,5.41997514710894,-1.86067981823474));
#26797=CARTESIAN_POINT('Ctrl Pts',(62.1764102940279,5.65231158284244,0.943203982060585));
#26798=CARTESIAN_POINT('Ctrl Pts',(62.7290418729753,4.52214419437993,3.51972610673135));
#26799=CARTESIAN_POINT('Ctrl Pts',(63.2816734519227,2.30190265343826,5.24780946258346));
#26800=CARTESIAN_POINT('Ctrl Pts',(63.8343050308701,-0.473218271369009,
5.71089524055341));
#26801=CARTESIAN_POINT('Ctrl Pts',(64.3869366098174,-3.13426874984932,4.79735545746814));
#26802=CARTESIAN_POINT('Ctrl Pts',(64.9395681887648,-5.03979591830014,2.72740115925714));
#26803=CARTESIAN_POINT('Ctrl Pts',(65.4921997677122,-5.73046769283071,2.96121409977839E-10));
#26804=CARTESIAN_POINT('Ctrl Pts',(66.0448313466595,-5.03979591868312,-2.72740116002078));
#26805=CARTESIAN_POINT('Ctrl Pts',(66.5974629256069,-3.13426874886167,-4.79735545609105));
#26806=CARTESIAN_POINT('Ctrl Pts',(67.1500945045543,-0.473218273533038,
-5.71089524334112));
#26807=CARTESIAN_POINT('Ctrl Pts',(67.7027260835016,2.30190265803138,-5.24780945677143));
#26808=CARTESIAN_POINT('Ctrl Pts',(68.255357662449,4.52214418469897,-3.51972611893208));
#26809=CARTESIAN_POINT('Ctrl Pts',(68.8079892413964,5.65231160321522,-0.943203956408587));
#26810=CARTESIAN_POINT('Ctrl Pts',(69.3606208203438,5.41997510425126,1.86067976428242));
#26811=CARTESIAN_POINT('Ctrl Pts',(69.9132523992911,3.88114025546219,4.21604221461142));
#26812=CARTESIAN_POINT('Ctrl Pts',(70.4658839782385,1.40674646354597,5.55511666690853));
#26813=CARTESIAN_POINT('Ctrl Pts',(71.0185155571859,-1.40674625429845,5.55511740772306));
#26814=CARTESIAN_POINT('Ctrl Pts',(71.5711471361332,-3.8811410043497,4.21604104496428));
#26815=CARTESIAN_POINT('Ctrl Pts',(72.1237787150806,-5.41997338236277,1.86068203981508));
#26816=CARTESIAN_POINT('Ctrl Pts',(72.676410294028,-5.65231529605741,-0.943208655172103));
#26817=CARTESIAN_POINT('Ctrl Pts',(73.2290418729754,-4.52213639346892,-3.51971627798694));
#26818=CARTESIAN_POINT('Ctrl Pts',(73.7816734519227,-2.30191914515453,-5.24783014539695));
#26819=CARTESIAN_POINT('Ctrl Pts',(74.3343050308701,0.473252278446422,-5.71085179682633));
#26820=CARTESIAN_POINT('Ctrl Pts',(74.8869366098175,3.13419106663809,-4.79744756259312));
#26821=CARTESIAN_POINT('Ctrl Pts',(75.4395681887648,5.03991467318512,-2.72720954086847));
#26822=CARTESIAN_POINT('Ctrl Pts',(75.8079892413964,5.49976642738082,-0.909403588662883));
#26823=CARTESIAN_POINT('Ctrl Pts',(75.9921997677122,5.49976642738082,-8.08232562162E-15));
#26824=CARTESIAN_POINT('',(75.9921997677122,5.49976642738082,-8.08232562162E-15));
#26825=CARTESIAN_POINT('',(33.9921997677122,5.49976642738082,0.));
#26826=CARTESIAN_POINT('Ctrl Pts',(75.9921997677122,5.49976642738082,-8.08232562162E-15));
#26827=CARTESIAN_POINT('Ctrl Pts',(75.8079892413964,5.49976642738082,-0.909403588662883));
#26828=CARTESIAN_POINT('Ctrl Pts',(75.4395681887648,5.03991467318512,-2.72720954086847));
#26829=CARTESIAN_POINT('Ctrl Pts',(74.8869366098175,3.13419106663809,-4.79744756259312));
#26830=CARTESIAN_POINT('Ctrl Pts',(74.3343050308701,0.473252278446422,-5.71085179682633));
#26831=CARTESIAN_POINT('Ctrl Pts',(73.7816734519227,-2.30191914515453,-5.24783014539695));
#26832=CARTESIAN_POINT('Ctrl Pts',(73.2290418729754,-4.52213639346892,-3.51971627798694));
#26833=CARTESIAN_POINT('Ctrl Pts',(72.676410294028,-5.65231529605741,-0.943208655172103));
#26834=CARTESIAN_POINT('Ctrl Pts',(72.1237787150806,-5.41997338236277,1.86068203981508));
#26835=CARTESIAN_POINT('Ctrl Pts',(71.5711471361332,-3.8811410043497,4.21604104496428));
#26836=CARTESIAN_POINT('Ctrl Pts',(71.0185155571859,-1.40674625429845,5.55511740772306));
#26837=CARTESIAN_POINT('Ctrl Pts',(70.4658839782385,1.40674646354597,5.55511666690853));
#26838=CARTESIAN_POINT('Ctrl Pts',(69.9132523992911,3.88114025546219,4.21604221461142));
#26839=CARTESIAN_POINT('Ctrl Pts',(69.3606208203438,5.41997510425126,1.86067976428242));
#26840=CARTESIAN_POINT('Ctrl Pts',(68.8079892413964,5.65231160321522,-0.943203956408587));
#26841=CARTESIAN_POINT('Ctrl Pts',(68.255357662449,4.52214418469897,-3.51972611893208));
#26842=CARTESIAN_POINT('Ctrl Pts',(67.7027260835016,2.30190265803138,-5.24780945677143));
#26843=CARTESIAN_POINT('Ctrl Pts',(67.1500945045543,-0.473218273533038,
-5.71089524334112));
#26844=CARTESIAN_POINT('Ctrl Pts',(66.5974629256069,-3.13426874886167,-4.79735545609105));
#26845=CARTESIAN_POINT('Ctrl Pts',(66.0448313466595,-5.03979591868312,-2.72740116002078));
#26846=CARTESIAN_POINT('Ctrl Pts',(65.4921997677122,-5.73046769283071,2.96121409977839E-10));
#26847=CARTESIAN_POINT('Ctrl Pts',(64.9395681887648,-5.03979591830014,2.72740115925714));
#26848=CARTESIAN_POINT('Ctrl Pts',(64.3869366098174,-3.13426874984932,4.79735545746814));
#26849=CARTESIAN_POINT('Ctrl Pts',(63.8343050308701,-0.473218271369009,
5.71089524055341));
#26850=CARTESIAN_POINT('Ctrl Pts',(63.2816734519227,2.30190265343826,5.24780946258346));
#26851=CARTESIAN_POINT('Ctrl Pts',(62.7290418729753,4.52214419437993,3.51972610673135));
#26852=CARTESIAN_POINT('Ctrl Pts',(62.1764102940279,5.65231158284244,0.943203982060585));
#26853=CARTESIAN_POINT('Ctrl Pts',(61.6237787150807,5.41997514710894,-1.86067981823474));
#26854=CARTESIAN_POINT('Ctrl Pts',(61.0711471361332,3.88114016531085,-4.21604210112775));
#26855=CARTESIAN_POINT('Ctrl Pts',(60.5185155571859,1.40674665317661,-5.55511690561524));
#26856=CARTESIAN_POINT('Ctrl Pts',(59.9658839782385,-1.40674665317677,-5.55511690561469));
#26857=CARTESIAN_POINT('Ctrl Pts',(59.4132523992911,-3.88114016531031,-4.2160421011286));
#26858=CARTESIAN_POINT('Ctrl Pts',(58.8606208203438,-5.4199751471102,-1.86067981823306));
#26859=CARTESIAN_POINT('Ctrl Pts',(58.3079892413963,-5.65231158283973,0.943203982057152));
#26860=CARTESIAN_POINT('Ctrl Pts',(57.755357662449,-4.52214419438564,3.51972610673854));
#26861=CARTESIAN_POINT('Ctrl Pts',(57.2027260835016,-2.30190265342626,5.24780946256833));
#26862=CARTESIAN_POINT('Ctrl Pts',(56.6500945045543,0.473218271343732,5.71089524058523));
#26863=CARTESIAN_POINT('Ctrl Pts',(56.0974629256069,3.13426874990249,4.79735545740121));
#26864=CARTESIAN_POINT('Ctrl Pts',(55.5448313466596,5.03979591818831,2.72740115939791));
#26865=CARTESIAN_POINT('Ctrl Pts',(54.9921997677122,5.73046769306595,-5.11805824213355E-15));
#26866=CARTESIAN_POINT('Ctrl Pts',(54.4395681887648,5.0397959181883,-2.72740115939791));
#26867=CARTESIAN_POINT('Ctrl Pts',(53.8869366098175,3.13426874990249,-4.79735545740122));
#26868=CARTESIAN_POINT('Ctrl Pts',(53.3343050308701,0.473218271343736,-5.71089524058523));
#26869=CARTESIAN_POINT('Ctrl Pts',(52.7816734519227,-2.30190265342625,-5.24780946256834));
#26870=CARTESIAN_POINT('Ctrl Pts',(52.2290418729753,-4.52214419438563,-3.51972610673855));
#26871=CARTESIAN_POINT('Ctrl Pts',(51.676410294028,-5.65231158283973,-0.943203982057156));
#26872=CARTESIAN_POINT('Ctrl Pts',(51.1237787150806,-5.4199751471102,1.86067981823306));
#26873=CARTESIAN_POINT('Ctrl Pts',(50.5711471361332,-3.8811401653103,4.2160421011286));
#26874=CARTESIAN_POINT('Ctrl Pts',(50.0185155571858,-1.40674665317677,5.5551169056147));
#26875=CARTESIAN_POINT('Ctrl Pts',(49.4658839782385,1.40674665317661,5.55511690561523));
#26876=CARTESIAN_POINT('Ctrl Pts',(48.9132523992911,3.88114016531086,4.21604210112774));
#26877=CARTESIAN_POINT('Ctrl Pts',(48.3606208203438,5.41997514710894,1.86067981823473));
#26878=CARTESIAN_POINT('Ctrl Pts',(47.8079892413964,5.65231158284243,-0.943203982060589));
#26879=CARTESIAN_POINT('Ctrl Pts',(47.255357662449,4.52214419437993,-3.51972610673135));
#26880=CARTESIAN_POINT('Ctrl Pts',(46.7027260835016,2.30190265343826,-5.24780946258346));
#26881=CARTESIAN_POINT('Ctrl Pts',(46.1500945045543,-0.473218271369011,
-5.71089524055342));
#26882=CARTESIAN_POINT('Ctrl Pts',(45.5974629256069,-3.13426874984933,-4.79735545746814));
#26883=CARTESIAN_POINT('Ctrl Pts',(45.0448313466595,-5.03979591830015,-2.72740115925713));
#26884=CARTESIAN_POINT('Ctrl Pts',(44.4921997677122,-5.73046769283071,-2.96113953592807E-10));
#26885=CARTESIAN_POINT('Ctrl Pts',(43.9395681887648,-5.03979591868312,2.72740116002078));
#26886=CARTESIAN_POINT('Ctrl Pts',(43.3869366098174,-3.13426874886167,4.79735545609104));
#26887=CARTESIAN_POINT('Ctrl Pts',(42.8343050308701,-0.473218273533045,
5.71089524334113));
#26888=CARTESIAN_POINT('Ctrl Pts',(42.2816734519227,2.30190265803137,5.24780945677143));
#26889=CARTESIAN_POINT('Ctrl Pts',(41.7290418729754,4.52214418469897,3.51972611893208));
#26890=CARTESIAN_POINT('Ctrl Pts',(41.1764102940279,5.65231160321522,0.943203956408585));
#26891=CARTESIAN_POINT('Ctrl Pts',(40.6237787150806,5.41997510425126,-1.86067976428242));
#26892=CARTESIAN_POINT('Ctrl Pts',(40.0711471361332,3.88114025546219,-4.21604221461142));
#26893=CARTESIAN_POINT('Ctrl Pts',(39.5185155571859,1.40674646354598,-5.55511666690852));
#26894=CARTESIAN_POINT('Ctrl Pts',(38.9658839782385,-1.40674625429844,-5.55511740772306));
#26895=CARTESIAN_POINT('Ctrl Pts',(38.4132523992911,-3.88114100434969,-4.2160410449643));
#26896=CARTESIAN_POINT('Ctrl Pts',(37.8606208203438,-5.41997338236277,-1.86068203981508));
#26897=CARTESIAN_POINT('Ctrl Pts',(37.3079892413964,-5.6523152960574,0.943208655172099));
#26898=CARTESIAN_POINT('Ctrl Pts',(36.755357662449,-4.52213639346893,3.51971627798693));
#26899=CARTESIAN_POINT('Ctrl Pts',(36.2027260835017,-2.30191914515453,5.24783014539696));
#26900=CARTESIAN_POINT('Ctrl Pts',(35.6500945045543,0.473252278446431,5.71085179682633));
#26901=CARTESIAN_POINT('Ctrl Pts',(35.0974629256069,3.13419106663809,4.79744756259311));
#26902=CARTESIAN_POINT('Ctrl Pts',(34.5448313466596,5.03991467318512,2.72720954086847));
#26903=CARTESIAN_POINT('Ctrl Pts',(34.176410294028,5.49976642738082,0.909403588662882));
#26904=CARTESIAN_POINT('Ctrl Pts',(33.9921997677122,5.49976642738082,0.));
#26905=CARTESIAN_POINT('',(74.9926516271063,5.5,-8.08266887437253E-15));
#26906=CARTESIAN_POINT('Ctrl Pts',(74.9926516271063,5.5,-8.88178419700125E-15));
#26907=CARTESIAN_POINT('Ctrl Pts',(74.9926516271063,5.49313135100536,-8.87169019419435E-15));
#26908=CARTESIAN_POINT('Ctrl Pts',(74.9928025594595,5.48616354876223,-8.85985100982881E-15));
#26909=CARTESIAN_POINT('Ctrl Pts',(74.9960623922239,5.41251939146685,-8.75162531201958E-15));
#26910=CARTESIAN_POINT('Ctrl Pts',(75.0129635856193,5.34674686927241,-8.64028104022342E-15));
#26911=CARTESIAN_POINT('Ctrl Pts',(75.0678279227212,5.23017858324776,-8.46897506618881E-15));
#26912=CARTESIAN_POINT('Ctrl Pts',(75.1045557576696,5.1784716444728,-8.3816878020062E-15));
#26913=CARTESIAN_POINT('Ctrl Pts',(75.2023392282651,5.08536492110004,-8.24486038109713E-15));
#26914=CARTESIAN_POINT('Ctrl Pts',(75.2593199555039,5.05418571732405,-7.68501720917694E-15));
#26915=CARTESIAN_POINT('Ctrl Pts',(75.3723346478213,5.01099405108005,-7.62154376619828E-15));
#26916=CARTESIAN_POINT('Ctrl Pts',(75.4380011585399,4.9992994690211,-7.59988681703217E-15));
#26917=CARTESIAN_POINT('Ctrl Pts',(75.5679318704974,5.00124746390966,-7.6027495438782E-15));
#26918=CARTESIAN_POINT('Ctrl Pts',(75.6303803662932,5.01468983699985,-7.77794865724713E-15));
#26919=CARTESIAN_POINT('Ctrl Pts',(75.7510076677018,5.06728521602235,-7.85524157233096E-15));
#26920=CARTESIAN_POINT('Ctrl Pts',(75.8069852154638,5.1062890809302,-7.92468346949603E-15));
#26921=CARTESIAN_POINT('Ctrl Pts',(75.8898187552,5.19148126768943,-8.0498798760885E-15));
#26922=CARTESIAN_POINT('Ctrl Pts',(75.9275855766847,5.24142762980879,-8.26790514855932E-15));
#26923=CARTESIAN_POINT('Ctrl Pts',(75.9798876154733,5.36745993607387,-8.45311922110734E-15));
#26924=CARTESIAN_POINT('Ctrl Pts',(75.992313334028,5.43375746391126,-8.78477899800761E-15));
#26925=CARTESIAN_POINT('Ctrl Pts',(75.9921997677122,5.49976642738082,-8.88178419700125E-15));
#26926=CARTESIAN_POINT('',(32.9926516271063,5.5,0.));
#26927=CARTESIAN_POINT('Ctrl Pts',(32.9926516271063,5.5,0.));
#26928=CARTESIAN_POINT('Ctrl Pts',(33.1768621534221,5.5,0.90940874905597));
#26929=CARTESIAN_POINT('Ctrl Pts',(33.5452832060536,5.0401165414414,2.72733561841164));
#26930=CARTESIAN_POINT('Ctrl Pts',(34.097914785001,3.13431992024721,4.79763437071315));
#26931=CARTESIAN_POINT('Ctrl Pts',(34.6505463639483,0.47327073373995,5.71108710593625));
#26932=CARTESIAN_POINT('Ctrl Pts',(35.2031779428958,-2.3020121722956,5.24804131697886));
#26933=CARTESIAN_POINT('Ctrl Pts',(35.7558095218431,-4.52232002588597,3.51985989359966));
#26934=CARTESIAN_POINT('Ctrl Pts',(36.3084411007905,-5.65254452743844,0.943246530010384));
#26935=CARTESIAN_POINT('Ctrl Pts',(36.8610726797378,-5.42019330761579,-1.86075734131042));
#26936=CARTESIAN_POINT('Ctrl Pts',(37.4137042586852,-3.88129844265893,-4.21621217675881));
#26937=CARTESIAN_POINT('Ctrl Pts',(37.9663358376326,-1.40680333428488,-5.55534273510501));
#26938=CARTESIAN_POINT('Ctrl Pts',(38.5189674165799,1.40680353896056,-5.55534205621606));
#26939=CARTESIAN_POINT('Ctrl Pts',(39.0715989955273,3.88129771013392,-4.21621324863341));
#26940=CARTESIAN_POINT('Ctrl Pts',(39.6242305744747,5.42019499188262,-1.86075525598994));
#26941=CARTESIAN_POINT('Ctrl Pts',(40.1768621534221,5.65254091528142,0.943242224042852));
#26942=CARTESIAN_POINT('Ctrl Pts',(40.7294937323694,4.52232764688486,3.51986891209907));
#26943=CARTESIAN_POINT('Ctrl Pts',(41.2821253113168,2.30199604540077,5.24802235924301));
#26944=CARTESIAN_POINT('Ctrl Pts',(41.8347568902642,-0.47323747180233,5.7111269323428));
#26945=CARTESIAN_POINT('Ctrl Pts',(42.3873884692115,-3.13439590518638,4.79755008340959));
#26946=CARTESIAN_POINT('Ctrl Pts',(42.9400200481589,-5.04000038161494,2.7275118097799));
#26947=CARTESIAN_POINT('Ctrl Pts',(43.4926516271062,-5.73070017611617,-2.71361235965901E-10));
#26948=CARTESIAN_POINT('Ctrl Pts',(44.0452832060537,-5.04000038124033,-2.72751180908009));
#26949=CARTESIAN_POINT('Ctrl Pts',(44.597914785001,-3.13439590615245,-4.79755008467159));
#26950=CARTESIAN_POINT('Ctrl Pts',(45.1505463639484,-0.473237469685579,
-5.71112692978812));
#26951=CARTESIAN_POINT('Ctrl Pts',(45.7031779428957,2.30199604090801,-5.2480223645692));
#26952=CARTESIAN_POINT('Ctrl Pts',(46.2558095218431,4.52232765635431,-3.5198689009182));
#26953=CARTESIAN_POINT('Ctrl Pts',(46.8084411007904,5.65254089535377,-0.943242247550575));
#26954=CARTESIAN_POINT('Ctrl Pts',(47.3610726797379,5.4201950338039,1.86075530543231));
#26955=CARTESIAN_POINT('Ctrl Pts',(47.9137042586852,3.88129762195231,4.21621314463597));
#26956=CARTESIAN_POINT('Ctrl Pts',(48.4663358376326,1.40680372444794,5.55534227496898));
#26957=CARTESIAN_POINT('Ctrl Pts',(49.0189674165799,-1.40680372444809,5.55534227496848));
#26958=CARTESIAN_POINT('Ctrl Pts',(49.5715989955273,-3.88129762195177,4.21621314463675));
#26959=CARTESIAN_POINT('Ctrl Pts',(50.1242305744747,-5.42019503380513,1.86075530543079));
#26960=CARTESIAN_POINT('Ctrl Pts',(50.6768621534221,-5.65254089535113,-0.943242247547429));
#26961=CARTESIAN_POINT('Ctrl Pts',(51.2294937323694,-4.52232765635988,-3.51986890092481));
#26962=CARTESIAN_POINT('Ctrl Pts',(51.7821253113168,-2.30199604089626,-5.24802236455534));
#26963=CARTESIAN_POINT('Ctrl Pts',(52.3347568902641,0.473237469660857,-5.71112692981728));
#26964=CARTESIAN_POINT('Ctrl Pts',(52.8873884692115,3.13439590620446,-4.79755008461025));
#26965=CARTESIAN_POINT('Ctrl Pts',(53.4400200481589,5.04000038113094,-2.7275118092091));
#26966=CARTESIAN_POINT('Ctrl Pts',(53.9926516271062,5.73070017634626,-5.09570864282292E-15));
#26967=CARTESIAN_POINT('Ctrl Pts',(54.5452832060537,5.04000038113094,2.7275118092091));
#26968=CARTESIAN_POINT('Ctrl Pts',(55.0979147850009,3.13439590620446,4.79755008461025));
#26969=CARTESIAN_POINT('Ctrl Pts',(55.6505463639484,0.473237469660853,5.71112692981727));
#26970=CARTESIAN_POINT('Ctrl Pts',(56.2031779428957,-2.30199604089627,5.24802236455534));
#26971=CARTESIAN_POINT('Ctrl Pts',(56.7558095218432,-4.52232765635989,3.5198689009248));
#26972=CARTESIAN_POINT('Ctrl Pts',(57.3084411007904,-5.65254089535113,0.943242247547423));
#26973=CARTESIAN_POINT('Ctrl Pts',(57.8610726797378,-5.42019503380513,-1.86075530543079));
#26974=CARTESIAN_POINT('Ctrl Pts',(58.4137042586852,-3.88129762195177,-4.21621314463675));
#26975=CARTESIAN_POINT('Ctrl Pts',(58.9663358376325,-1.4068037244481,-5.55534227496848));
#26976=CARTESIAN_POINT('Ctrl Pts',(59.51896741658,1.40680372444794,-5.55534227496898));
#26977=CARTESIAN_POINT('Ctrl Pts',(60.0715989955273,3.88129762195231,-4.21621314463597));
#26978=CARTESIAN_POINT('Ctrl Pts',(60.6242305744747,5.4201950338039,-1.86075530543232));
#26979=CARTESIAN_POINT('Ctrl Pts',(61.176862153422,5.65254089535377,0.94324224755057));
#26980=CARTESIAN_POINT('Ctrl Pts',(61.7294937323694,4.52232765635431,3.5198689009182));
#26981=CARTESIAN_POINT('Ctrl Pts',(62.2821253113167,2.30199604090801,5.2480223645692));
#26982=CARTESIAN_POINT('Ctrl Pts',(62.8347568902642,-0.473237469685578,
5.71112692978812));
#26983=CARTESIAN_POINT('Ctrl Pts',(63.3873884692115,-3.13439590615245,4.79755008467159));
#26984=CARTESIAN_POINT('Ctrl Pts',(63.9400200481589,-5.04000038124033,2.7275118090801));
#26985=CARTESIAN_POINT('Ctrl Pts',(64.4926516271063,-5.73070017611617,2.71368745431234E-10));
#26986=CARTESIAN_POINT('Ctrl Pts',(65.0452832060536,-5.04000038161494,-2.7275118097799));
#26987=CARTESIAN_POINT('Ctrl Pts',(65.597914785001,-3.13439590518638,-4.7975500834096));
#26988=CARTESIAN_POINT('Ctrl Pts',(66.1505463639483,-0.473237471802323,
-5.7111269323428));
#26989=CARTESIAN_POINT('Ctrl Pts',(66.7031779428957,2.30199604540077,-5.248022359243));
#26990=CARTESIAN_POINT('Ctrl Pts',(67.255809521843,4.52232764688486,-3.51986891209906));
#26991=CARTESIAN_POINT('Ctrl Pts',(67.8084411007905,5.65254091528143,-0.943242224042853));
#26992=CARTESIAN_POINT('Ctrl Pts',(68.3610726797379,5.42019499188262,1.86075525598994));
#26993=CARTESIAN_POINT('Ctrl Pts',(68.9137042586851,3.88129771013392,4.21621324863341));
#26994=CARTESIAN_POINT('Ctrl Pts',(69.4663358376326,1.40680353896055,5.55534205621606));
#26995=CARTESIAN_POINT('Ctrl Pts',(70.0189674165799,-1.4068033342849,5.55534273510501));
#26996=CARTESIAN_POINT('Ctrl Pts',(70.5715989955273,-3.88129844265893,4.21621217675881));
#26997=CARTESIAN_POINT('Ctrl Pts',(71.1242305744747,-5.42019330761579,1.86075734131042));
#26998=CARTESIAN_POINT('Ctrl Pts',(71.6768621534221,-5.65254452743844,-0.943246530010386));
#26999=CARTESIAN_POINT('Ctrl Pts',(72.2294937323694,-4.52232002588597,-3.51985989359967));
#27000=CARTESIAN_POINT('Ctrl Pts',(72.7821253113168,-2.3020121722956,-5.24804131697885));
#27001=CARTESIAN_POINT('Ctrl Pts',(73.3347568902641,0.47327073373994,-5.71108710593626));
#27002=CARTESIAN_POINT('Ctrl Pts',(73.8873884692115,3.13431992024721,-4.79763437071315));
#27003=CARTESIAN_POINT('Ctrl Pts',(74.4400200481589,5.04011654144139,-2.72733561841164));
#27004=CARTESIAN_POINT('Ctrl Pts',(74.8084411007905,5.5,-0.909408749055971));
#27005=CARTESIAN_POINT('Ctrl Pts',(74.9926516271063,5.5,-8.08266887437253E-15));
#27006=CARTESIAN_POINT('Ctrl Pts',(32.9926516271063,5.5,-1.33481475863792E-22));
#27007=CARTESIAN_POINT('Ctrl Pts',(32.9926516271063,5.49313135093644,-1.33481475863792E-22));
#27008=CARTESIAN_POINT('Ctrl Pts',(32.9928025594625,5.48616354862232,0.));
#27009=CARTESIAN_POINT('Ctrl Pts',(32.9960623922631,5.41251939125576,0.));
#27010=CARTESIAN_POINT('Ctrl Pts',(33.012963585686,5.34674686906042,0.));
#27011=CARTESIAN_POINT('Ctrl Pts',(33.0678279228392,5.23017858306288,0.));
#27012=CARTESIAN_POINT('Ctrl Pts',(33.1045557578012,5.17847164431084,0.));
#27013=CARTESIAN_POINT('Ctrl Pts',(33.202339228433,5.08536492098311,0.));
#27014=CARTESIAN_POINT('Ctrl Pts',(33.2593199556946,5.054185717226,0.));
#27015=CARTESIAN_POINT('Ctrl Pts',(33.3723346480206,5.01099405103351,0.));
#27016=CARTESIAN_POINT('Ctrl Pts',(33.4380011587359,4.99929946899863,0.));
#27017=CARTESIAN_POINT('Ctrl Pts',(33.5679318706913,5.0012474639378,0.));
#27018=CARTESIAN_POINT('Ctrl Pts',(33.6303803664784,5.01468983705302,0.));
#27019=CARTESIAN_POINT('Ctrl Pts',(33.75100766786,5.06728521611982,0.));
#27020=CARTESIAN_POINT('Ctrl Pts',(33.8069852156061,5.10628908104261,0.));
#27021=CARTESIAN_POINT('Ctrl Pts',(33.8898187553161,5.19148126783547,0.));
#27022=CARTESIAN_POINT('Ctrl Pts',(33.9275855767874,5.24142762997304,0.));
#27023=CARTESIAN_POINT('Ctrl Pts',(33.9798876154972,5.36745993620988,0.));
#27024=CARTESIAN_POINT('Ctrl Pts',(33.9923133340279,5.4337574639749,5.17361254957654E-35));
#27025=CARTESIAN_POINT('Ctrl Pts',(33.9921997677122,5.49976642738082,5.17361254957654E-35));
#27026=CARTESIAN_POINT('Ctrl Pts',(33.9921997677122,5.49976642738082,0.));
#27027=CARTESIAN_POINT('Ctrl Pts',(34.176410294028,5.49976642738082,0.909403588662882));
#27028=CARTESIAN_POINT('Ctrl Pts',(34.5448313466596,5.03991467318512,2.72720954086847));
#27029=CARTESIAN_POINT('Ctrl Pts',(35.0974629256069,3.13419106663809,4.79744756259311));
#27030=CARTESIAN_POINT('Ctrl Pts',(35.6500945045543,0.473252278446431,5.71085179682633));
#27031=CARTESIAN_POINT('Ctrl Pts',(36.2027260835017,-2.30191914515453,5.24783014539696));
#27032=CARTESIAN_POINT('Ctrl Pts',(36.755357662449,-4.52213639346893,3.51971627798693));
#27033=CARTESIAN_POINT('Ctrl Pts',(37.3079892413964,-5.6523152960574,0.943208655172099));
#27034=CARTESIAN_POINT('Ctrl Pts',(37.8606208203438,-5.41997338236277,-1.86068203981508));
#27035=CARTESIAN_POINT('Ctrl Pts',(38.4132523992911,-3.88114100434969,-4.2160410449643));
#27036=CARTESIAN_POINT('Ctrl Pts',(38.9658839782385,-1.40674625429844,-5.55511740772306));
#27037=CARTESIAN_POINT('Ctrl Pts',(39.5185155571859,1.40674646354598,-5.55511666690852));
#27038=CARTESIAN_POINT('Ctrl Pts',(40.0711471361332,3.88114025546219,-4.21604221461142));
#27039=CARTESIAN_POINT('Ctrl Pts',(40.6237787150806,5.41997510425126,-1.86067976428242));
#27040=CARTESIAN_POINT('Ctrl Pts',(41.1764102940279,5.65231160321522,0.943203956408585));
#27041=CARTESIAN_POINT('Ctrl Pts',(41.7290418729754,4.52214418469897,3.51972611893208));
#27042=CARTESIAN_POINT('Ctrl Pts',(42.2816734519227,2.30190265803137,5.24780945677143));
#27043=CARTESIAN_POINT('Ctrl Pts',(42.8343050308701,-0.473218273533045,
5.71089524334113));
#27044=CARTESIAN_POINT('Ctrl Pts',(43.3869366098174,-3.13426874886167,4.79735545609104));
#27045=CARTESIAN_POINT('Ctrl Pts',(43.9395681887648,-5.03979591868312,2.72740116002078));
#27046=CARTESIAN_POINT('Ctrl Pts',(44.4921997677122,-5.73046769283071,-2.96113953592807E-10));
#27047=CARTESIAN_POINT('Ctrl Pts',(45.0448313466595,-5.03979591830015,-2.72740115925713));
#27048=CARTESIAN_POINT('Ctrl Pts',(45.5974629256069,-3.13426874984933,-4.79735545746814));
#27049=CARTESIAN_POINT('Ctrl Pts',(46.1500945045543,-0.473218271369011,
-5.71089524055342));
#27050=CARTESIAN_POINT('Ctrl Pts',(46.7027260835016,2.30190265343826,-5.24780946258346));
#27051=CARTESIAN_POINT('Ctrl Pts',(47.255357662449,4.52214419437993,-3.51972610673135));
#27052=CARTESIAN_POINT('Ctrl Pts',(47.8079892413964,5.65231158284243,-0.943203982060589));
#27053=CARTESIAN_POINT('Ctrl Pts',(48.3606208203438,5.41997514710894,1.86067981823473));
#27054=CARTESIAN_POINT('Ctrl Pts',(48.9132523992911,3.88114016531086,4.21604210112774));
#27055=CARTESIAN_POINT('Ctrl Pts',(49.4658839782385,1.40674665317661,5.55511690561523));
#27056=CARTESIAN_POINT('Ctrl Pts',(50.0185155571858,-1.40674665317677,5.5551169056147));
#27057=CARTESIAN_POINT('Ctrl Pts',(50.5711471361332,-3.8811401653103,4.2160421011286));
#27058=CARTESIAN_POINT('Ctrl Pts',(51.1237787150806,-5.4199751471102,1.86067981823306));
#27059=CARTESIAN_POINT('Ctrl Pts',(51.676410294028,-5.65231158283973,-0.943203982057156));
#27060=CARTESIAN_POINT('Ctrl Pts',(52.2290418729753,-4.52214419438563,-3.51972610673855));
#27061=CARTESIAN_POINT('Ctrl Pts',(52.7816734519227,-2.30190265342625,-5.24780946256834));
#27062=CARTESIAN_POINT('Ctrl Pts',(53.3343050308701,0.473218271343736,-5.71089524058523));
#27063=CARTESIAN_POINT('Ctrl Pts',(53.8869366098175,3.13426874990249,-4.79735545740122));
#27064=CARTESIAN_POINT('Ctrl Pts',(54.4395681887648,5.0397959181883,-2.72740115939791));
#27065=CARTESIAN_POINT('Ctrl Pts',(54.9921997677122,5.73046769306595,-5.11805824213355E-15));
#27066=CARTESIAN_POINT('Ctrl Pts',(55.5448313466596,5.03979591818831,2.72740115939791));
#27067=CARTESIAN_POINT('Ctrl Pts',(56.0974629256069,3.13426874990249,4.79735545740121));
#27068=CARTESIAN_POINT('Ctrl Pts',(56.6500945045543,0.473218271343732,5.71089524058523));
#27069=CARTESIAN_POINT('Ctrl Pts',(57.2027260835016,-2.30190265342626,5.24780946256833));
#27070=CARTESIAN_POINT('Ctrl Pts',(57.755357662449,-4.52214419438564,3.51972610673854));
#27071=CARTESIAN_POINT('Ctrl Pts',(58.3079892413963,-5.65231158283973,0.943203982057152));
#27072=CARTESIAN_POINT('Ctrl Pts',(58.8606208203438,-5.4199751471102,-1.86067981823306));
#27073=CARTESIAN_POINT('Ctrl Pts',(59.4132523992911,-3.88114016531031,-4.2160421011286));
#27074=CARTESIAN_POINT('Ctrl Pts',(59.9658839782385,-1.40674665317677,-5.55511690561469));
#27075=CARTESIAN_POINT('Ctrl Pts',(60.5185155571859,1.40674665317661,-5.55511690561524));
#27076=CARTESIAN_POINT('Ctrl Pts',(61.0711471361332,3.88114016531085,-4.21604210112775));
#27077=CARTESIAN_POINT('Ctrl Pts',(61.6237787150807,5.41997514710894,-1.86067981823474));
#27078=CARTESIAN_POINT('Ctrl Pts',(62.1764102940279,5.65231158284244,0.943203982060585));
#27079=CARTESIAN_POINT('Ctrl Pts',(62.7290418729753,4.52214419437993,3.51972610673135));
#27080=CARTESIAN_POINT('Ctrl Pts',(63.2816734519227,2.30190265343826,5.24780946258346));
#27081=CARTESIAN_POINT('Ctrl Pts',(63.8343050308701,-0.473218271369009,
5.71089524055341));
#27082=CARTESIAN_POINT('Ctrl Pts',(64.3869366098174,-3.13426874984932,4.79735545746814));
#27083=CARTESIAN_POINT('Ctrl Pts',(64.9395681887648,-5.03979591830014,2.72740115925714));
#27084=CARTESIAN_POINT('Ctrl Pts',(65.4921997677122,-5.73046769283071,2.96121409977839E-10));
#27085=CARTESIAN_POINT('Ctrl Pts',(66.0448313466595,-5.03979591868312,-2.72740116002078));
#27086=CARTESIAN_POINT('Ctrl Pts',(66.5974629256069,-3.13426874886167,-4.79735545609105));
#27087=CARTESIAN_POINT('Ctrl Pts',(67.1500945045543,-0.473218273533038,
-5.71089524334112));
#27088=CARTESIAN_POINT('Ctrl Pts',(67.7027260835016,2.30190265803138,-5.24780945677143));
#27089=CARTESIAN_POINT('Ctrl Pts',(68.255357662449,4.52214418469897,-3.51972611893208));
#27090=CARTESIAN_POINT('Ctrl Pts',(68.8079892413964,5.65231160321522,-0.943203956408587));
#27091=CARTESIAN_POINT('Ctrl Pts',(69.3606208203438,5.41997510425126,1.86067976428242));
#27092=CARTESIAN_POINT('Ctrl Pts',(69.9132523992911,3.88114025546219,4.21604221461142));
#27093=CARTESIAN_POINT('Ctrl Pts',(70.4658839782385,1.40674646354597,5.55511666690853));
#27094=CARTESIAN_POINT('Ctrl Pts',(71.0185155571859,-1.40674625429845,5.55511740772306));
#27095=CARTESIAN_POINT('Ctrl Pts',(71.5711471361332,-3.8811410043497,4.21604104496428));
#27096=CARTESIAN_POINT('Ctrl Pts',(72.1237787150806,-5.41997338236277,1.86068203981508));
#27097=CARTESIAN_POINT('Ctrl Pts',(72.676410294028,-5.65231529605741,-0.943208655172103));
#27098=CARTESIAN_POINT('Ctrl Pts',(73.2290418729754,-4.52213639346892,-3.51971627798694));
#27099=CARTESIAN_POINT('Ctrl Pts',(73.7816734519227,-2.30191914515453,-5.24783014539695));
#27100=CARTESIAN_POINT('Ctrl Pts',(74.3343050308701,0.473252278446422,-5.71085179682633));
#27101=CARTESIAN_POINT('Ctrl Pts',(74.8869366098175,3.13419106663809,-4.79744756259312));
#27102=CARTESIAN_POINT('Ctrl Pts',(75.4395681887648,5.03991467318512,-2.72720954086847));
#27103=CARTESIAN_POINT('Ctrl Pts',(75.8079892413964,5.49976642738082,-0.909403588662883));
#27104=CARTESIAN_POINT('Ctrl Pts',(75.9921997677122,5.49976642738082,-8.08232562162E-15));
#27105=CARTESIAN_POINT('Ctrl Pts',(33.9920707665653,5.57474668825,0.));
#27106=CARTESIAN_POINT('Ctrl Pts',(34.1762812928811,5.57474668825,0.921801519276635));
#27107=CARTESIAN_POINT('Ctrl Pts',(34.5447023455127,5.10862550688029,2.76439064201748));
#27108=CARTESIAN_POINT('Ctrl Pts',(35.0973339244601,3.17692056506673,4.86285271511581));
#27109=CARTESIAN_POINT('Ctrl Pts',(35.6499655034074,0.479704279887822,5.78870979651738));
#27110=CARTESIAN_POINT('Ctrl Pts',(36.2025970823548,-2.33330198195422,5.31937556836421));
#27111=CARTESIAN_POINT('Ctrl Pts',(36.7552286613021,-4.5837882052994,3.56770176400508));
#27112=CARTESIAN_POINT('Ctrl Pts',(37.3078602402495,-5.72937521578602,0.956067733435914));
#27113=CARTESIAN_POINT('Ctrl Pts',(37.8604918191969,-5.49386570747434,-1.88604934388851));
#27114=CARTESIAN_POINT('Ctrl Pts',(38.4131233981442,-3.93405390825201,-4.27351975497624));
#27115=CARTESIAN_POINT('Ctrl Pts',(38.9657549770916,-1.42592490042418,-5.63085219620485));
#27116=CARTESIAN_POINT('Ctrl Pts',(39.518386556039,1.42592511248475,-5.63085144582777));
#27117=CARTESIAN_POINT('Ctrl Pts',(40.0710181349864,3.93405314929682,-4.27352093972135));
#27118=CARTESIAN_POINT('Ctrl Pts',(40.6236497139337,5.4938674525111,-1.8860470389829));
#27119=CARTESIAN_POINT('Ctrl Pts',(41.176281292881,5.729371473299,0.95606297402021));
#27120=CARTESIAN_POINT('Ctrl Pts',(41.7289128718285,4.58379610127107,3.56771173198016));
#27121=CARTESIAN_POINT('Ctrl Pts',(42.2815444507758,2.33328527318593,5.31935461269972));
#27122=CARTESIAN_POINT('Ctrl Pts',(42.8341760297232,-0.479669817828385,
5.78875380394745));
#27123=CARTESIAN_POINT('Ctrl Pts',(43.3868076086705,-3.17699929161356,4.8627594207284));
#27124=CARTESIAN_POINT('Ctrl Pts',(43.9394391876179,-5.10850515589866,2.76458473973461));
#27125=CARTESIAN_POINT('Ctrl Pts',(44.4920707665653,-5.80859309124294,-2.99936115018113E-10));
#27126=CARTESIAN_POINT('Ctrl Pts',(45.0447023455126,-5.10850515551054,-2.7645847389611));
#27127=CARTESIAN_POINT('Ctrl Pts',(45.59733392446,-3.17699929261449,-4.86275942212328));
#27128=CARTESIAN_POINT('Ctrl Pts',(46.1499655034074,-0.479669815635259,
-5.78875380112376));
#27129=CARTESIAN_POINT('Ctrl Pts',(46.7025970823548,2.33328526853108,-5.31935461858677));
#27130=CARTESIAN_POINT('Ctrl Pts',(47.2552286613021,4.58379611108217,-3.56771171962194));
#27131=CARTESIAN_POINT('Ctrl Pts',(47.8078602402495,5.72937145265234,-0.956063000003334));
#27132=CARTESIAN_POINT('Ctrl Pts',(48.3604918191969,5.49386749594493,1.88604709363163));
#27133=CARTESIAN_POINT('Ctrl Pts',(48.9131233981442,3.93405305793353,4.27352082477281));
#27134=CARTESIAN_POINT('Ctrl Pts',(49.4657549770916,1.42592530466468,5.63085168761574));
#27135=CARTESIAN_POINT('Ctrl Pts',(50.018386556039,-1.42592530466484,5.6308516876152));
#27136=CARTESIAN_POINT('Ctrl Pts',(50.5710181349864,-3.93405305793297,4.27352082477367));
#27137=CARTESIAN_POINT('Ctrl Pts',(51.1236497139337,-5.49386749594621,1.88604709362994));
#27138=CARTESIAN_POINT('Ctrl Pts',(51.6762812928811,-5.7293714526496,-0.956062999999857));
#27139=CARTESIAN_POINT('Ctrl Pts',(52.2289128718284,-4.58379611108795,-3.56771171962923));
#27140=CARTESIAN_POINT('Ctrl Pts',(52.7815444507759,-2.3332852685189,-5.31935461857145));
#27141=CARTESIAN_POINT('Ctrl Pts',(53.3341760297232,0.479669815609644,-5.78875380115598));
#27142=CARTESIAN_POINT('Ctrl Pts',(53.8868076086706,3.17699929266837,-4.86275942205549));
#27143=CARTESIAN_POINT('Ctrl Pts',(54.4394391876179,5.10850515539719,-2.7645847391037));
#27144=CARTESIAN_POINT('Ctrl Pts',(54.9920707665653,5.80859309148135,-5.41419043299935E-15));
#27145=CARTESIAN_POINT('Ctrl Pts',(55.5447023455127,5.1085051553972,2.7645847391037));
#27146=CARTESIAN_POINT('Ctrl Pts',(56.0973339244601,3.17699929266837,4.86275942205548));
#27147=CARTESIAN_POINT('Ctrl Pts',(56.6499655034074,0.47966981560964,5.78875380115598));
#27148=CARTESIAN_POINT('Ctrl Pts',(57.2025970823548,-2.33328526851891,5.31935461857144));
#27149=CARTESIAN_POINT('Ctrl Pts',(57.7552286613021,-4.58379611108796,3.56771171962922));
#27150=CARTESIAN_POINT('Ctrl Pts',(58.3078602402495,-5.7293714526496,0.956062999999852));
#27151=CARTESIAN_POINT('Ctrl Pts',(58.8604918191969,-5.49386749594621,-1.88604709362995));
#27152=CARTESIAN_POINT('Ctrl Pts',(59.4131233981442,-3.93405305793297,-4.27352082477368));
#27153=CARTESIAN_POINT('Ctrl Pts',(59.9657549770916,-1.42592530466484,-5.63085168761519));
#27154=CARTESIAN_POINT('Ctrl Pts',(60.518386556039,1.42592530466468,-5.63085168761575));
#27155=CARTESIAN_POINT('Ctrl Pts',(61.0710181349863,3.93405305793353,-4.27352082477281));
#27156=CARTESIAN_POINT('Ctrl Pts',(61.6236497139338,5.49386749594494,-1.88604709363164));
#27157=CARTESIAN_POINT('Ctrl Pts',(62.1762812928811,5.72937145265234,0.95606300000333));
#27158=CARTESIAN_POINT('Ctrl Pts',(62.7289128718285,4.58379611108217,3.56771171962194));
#27159=CARTESIAN_POINT('Ctrl Pts',(63.2815444507758,2.33328526853108,5.31935461858677));
#27160=CARTESIAN_POINT('Ctrl Pts',(63.8341760297232,-0.479669815635258,
5.78875380112375));
#27161=CARTESIAN_POINT('Ctrl Pts',(64.3868076086705,-3.17699929261449,4.86275942212328));
#27162=CARTESIAN_POINT('Ctrl Pts',(64.9394391876179,-5.10850515551053,2.76458473896111));
#27163=CARTESIAN_POINT('Ctrl Pts',(65.4920707665653,-5.80859309124295,2.9994369153224E-10));
#27164=CARTESIAN_POINT('Ctrl Pts',(66.0447023455127,-5.10850515589866,-2.76458473973461));
#27165=CARTESIAN_POINT('Ctrl Pts',(66.59733392446,-3.17699929161356,-4.86275942072841));
#27166=CARTESIAN_POINT('Ctrl Pts',(67.1499655034074,-0.479669817828379,
-5.78875380394745));
#27167=CARTESIAN_POINT('Ctrl Pts',(67.7025970823548,2.33328527318594,-5.31935461269972));
#27168=CARTESIAN_POINT('Ctrl Pts',(68.2552286613022,4.58379610127107,-3.56771173198016));
#27169=CARTESIAN_POINT('Ctrl Pts',(68.8078602402495,5.72937147329901,-0.956062974020212));
#27170=CARTESIAN_POINT('Ctrl Pts',(69.3604918191969,5.4938674525111,1.8860470389829));
#27171=CARTESIAN_POINT('Ctrl Pts',(69.9131233981443,3.93405314929682,4.27352093972134));
#27172=CARTESIAN_POINT('Ctrl Pts',(70.4657549770917,1.42592511248473,5.63085144582777));
#27173=CARTESIAN_POINT('Ctrl Pts',(71.018386556039,-1.42592490042419,5.63085219620485));
#27174=CARTESIAN_POINT('Ctrl Pts',(71.5710181349864,-3.93405390825202,4.27351975497623));
#27175=CARTESIAN_POINT('Ctrl Pts',(72.1236497139337,-5.49386570747434,1.88604934388851));
#27176=CARTESIAN_POINT('Ctrl Pts',(72.6762812928811,-5.72937521578603,-0.956067733435918));
#27177=CARTESIAN_POINT('Ctrl Pts',(73.2289128718285,-4.58378820529939,-3.56770176400509));
#27178=CARTESIAN_POINT('Ctrl Pts',(73.7815444507758,-2.33330198195422,-5.31937556836421));
#27179=CARTESIAN_POINT('Ctrl Pts',(74.3341760297232,0.479704279887813,-5.78870979651738));
#27180=CARTESIAN_POINT('Ctrl Pts',(74.8868076086706,3.17692056506672,-4.86285271511582));
#27181=CARTESIAN_POINT('Ctrl Pts',(75.4394391876179,5.10862550688029,-2.76439064201748));
#27182=CARTESIAN_POINT('Ctrl Pts',(75.8078602402495,5.57474668825,-0.921801519276636));
#27183=CARTESIAN_POINT('Ctrl Pts',(75.9920707665653,5.57474668825,-8.19251482538721E-15));
#27184=CARTESIAN_POINT('Ctrl Pts',(33.9431414536155,5.79981109503712,0.));
#27185=CARTESIAN_POINT('Ctrl Pts',(34.1273519799313,5.79981109503712,0.95899747143683));
#27186=CARTESIAN_POINT('Ctrl Pts',(34.4957730325629,5.31486464408031,2.87600085013837));
#27187=CARTESIAN_POINT('Ctrl Pts',(35.0484046115103,3.30517718677737,5.05916675657821));
#27188=CARTESIAN_POINT('Ctrl Pts',(35.6010361904576,0.499070024096898,6.02240821551781));
#27189=CARTESIAN_POINT('Ctrl Pts',(36.153667769405,-2.42749964852484,5.53412340547436));
#27190=CARTESIAN_POINT('Ctrl Pts',(36.7062993483523,-4.76884068918239,3.71173413415615));
#27191=CARTESIAN_POINT('Ctrl Pts',(37.2589309272997,-5.96067611682369,0.994664977192594));
#27192=CARTESIAN_POINT('Ctrl Pts',(37.8115625062471,-5.71565890873659,-1.96219104782992));
#27193=CARTESIAN_POINT('Ctrl Pts',(38.3641940851944,-4.09287582201278,-4.4460463256512));
#27194=CARTESIAN_POINT('Ctrl Pts',(38.9168256641418,-1.48349100436533,-5.85817564103365));
#27195=CARTESIAN_POINT('Ctrl Pts',(39.4694572430892,1.48349122236704,-5.85817489580175));
#27196=CARTESIAN_POINT('Ctrl Pts',(40.0220888220366,4.09287504179451,-4.44604750227257));
#27197=CARTESIAN_POINT('Ctrl Pts',(40.5747204009839,5.71566070266274,-1.96218875872725));
#27198=CARTESIAN_POINT('Ctrl Pts',(41.1273519799312,5.96067226948622,0.994660250423079));
#27199=CARTESIAN_POINT('Ctrl Pts',(41.6799835588787,4.76884880636957,3.71174403388056));
#27200=CARTESIAN_POINT('Ctrl Pts',(42.232615137826,2.42748247163953,5.5341025943587));
#27201=CARTESIAN_POINT('Ctrl Pts',(42.7852467167734,-0.499034596539813,
6.0224519278597));
#27202=CARTESIAN_POINT('Ctrl Pts',(43.3378782957207,-3.30525811894677,5.0590741705265));
#27203=CARTESIAN_POINT('Ctrl Pts',(43.8905098746681,-5.31474092131558,2.87619395462708));
#27204=CARTESIAN_POINT('Ctrl Pts',(44.4431414536155,-6.04309214833711,-2.97879057897562E-10));
#27205=CARTESIAN_POINT('Ctrl Pts',(44.9957730325628,-5.31474092091659,-2.87619395385888));
#27206=CARTESIAN_POINT('Ctrl Pts',(45.5484046115102,-3.30525811997574,-5.05907417191182));
#27207=CARTESIAN_POINT('Ctrl Pts',(46.1010361904576,-0.499034594285245,
-6.02245192505537));
#27208=CARTESIAN_POINT('Ctrl Pts',(46.653667769405,2.42748246685427,-5.53410260020539));
#27209=CARTESIAN_POINT('Ctrl Pts',(47.2062993483523,4.76884881645555,-3.71174402160707));
#27210=CARTESIAN_POINT('Ctrl Pts',(47.7589309272997,5.96067224826112,-0.994660276228043));
#27211=CARTESIAN_POINT('Ctrl Pts',(48.3115625062471,5.71566074731342,1.96218881300126));
#27212=CARTESIAN_POINT('Ctrl Pts',(48.8641940851944,4.09287494787157,4.44604738811221));
#27213=CARTESIAN_POINT('Ctrl Pts',(49.4168256641418,1.48349141993114,5.85817513593182));
#27214=CARTESIAN_POINT('Ctrl Pts',(49.9694572430891,-1.48349141993129,5.85817513593129));
#27215=CARTESIAN_POINT('Ctrl Pts',(50.5220888220366,-4.09287494787099,4.44604738811307));
#27216=CARTESIAN_POINT('Ctrl Pts',(51.0747204009839,-5.71566074731474,1.96218881299959));
#27217=CARTESIAN_POINT('Ctrl Pts',(51.6273519799313,-5.96067224825831,-0.994660276224589));
#27218=CARTESIAN_POINT('Ctrl Pts',(52.1799835588786,-4.76884881646149,-3.71174402161432));
#27219=CARTESIAN_POINT('Ctrl Pts',(52.7326151378261,-2.42748246684175,-5.53410260019018));
#27220=CARTESIAN_POINT('Ctrl Pts',(53.2852467167734,0.499034594258913,-6.02245192508737));
#27221=CARTESIAN_POINT('Ctrl Pts',(53.8378782957208,3.30525812003113,-5.0590741718445));
#27222=CARTESIAN_POINT('Ctrl Pts',(54.3905098746681,5.31474092080006,-2.8761939540005));
#27223=CARTESIAN_POINT('Ctrl Pts',(54.9431414536155,6.0430921485822,-6.36963580352865E-15));
#27224=CARTESIAN_POINT('Ctrl Pts',(55.4957730325629,5.31474092080007,2.8761939540005));
#27225=CARTESIAN_POINT('Ctrl Pts',(56.0484046115103,3.30525812003113,5.05907417184449));
#27226=CARTESIAN_POINT('Ctrl Pts',(56.6010361904576,0.499034594258907,6.02245192508737));
#27227=CARTESIAN_POINT('Ctrl Pts',(57.1536677694049,-2.42748246684176,5.53410260019017));
#27228=CARTESIAN_POINT('Ctrl Pts',(57.7062993483523,-4.7688488164615,3.71174402161431));
#27229=CARTESIAN_POINT('Ctrl Pts',(58.2589309272996,-5.9606722482583,0.994660276224585));
#27230=CARTESIAN_POINT('Ctrl Pts',(58.8115625062471,-5.71566074731474,-1.96218881299959));
#27231=CARTESIAN_POINT('Ctrl Pts',(59.3641940851944,-4.09287494787099,-4.44604738811308));
#27232=CARTESIAN_POINT('Ctrl Pts',(59.9168256641418,-1.4834914199313,-5.85817513593128));
#27233=CARTESIAN_POINT('Ctrl Pts',(60.4694572430892,1.48349141993113,-5.85817513593183));
#27234=CARTESIAN_POINT('Ctrl Pts',(61.0220888220365,4.09287494787156,-4.44604738811222));
#27235=CARTESIAN_POINT('Ctrl Pts',(61.574720400984,5.71566074731343,-1.96218881300128));
#27236=CARTESIAN_POINT('Ctrl Pts',(62.1273519799312,5.96067224826113,0.994660276228038));
#27237=CARTESIAN_POINT('Ctrl Pts',(62.6799835588787,4.76884881645555,3.71174402160707));
#27238=CARTESIAN_POINT('Ctrl Pts',(63.232615137826,2.42748246685427,5.53410260020538));
#27239=CARTESIAN_POINT('Ctrl Pts',(63.7852467167734,-0.499034594285243,
6.02245192505537));
#27240=CARTESIAN_POINT('Ctrl Pts',(64.3378782957207,-3.30525811997573,5.05907417191182));
#27241=CARTESIAN_POINT('Ctrl Pts',(64.8905098746681,-5.31474092091658,2.87619395385889));
#27242=CARTESIAN_POINT('Ctrl Pts',(65.4431414536155,-6.04309214833712,2.97887036704478E-10));
#27243=CARTESIAN_POINT('Ctrl Pts',(65.9957730325628,-5.31474092131558,-2.87619395462708));
#27244=CARTESIAN_POINT('Ctrl Pts',(66.5484046115102,-3.30525811894677,-5.05907417052651));
#27245=CARTESIAN_POINT('Ctrl Pts',(67.1010361904576,-0.499034596539806,
-6.0224519278597));
#27246=CARTESIAN_POINT('Ctrl Pts',(67.653667769405,2.42748247163954,-5.5341025943587));
#27247=CARTESIAN_POINT('Ctrl Pts',(68.2062993483523,4.76884880636957,-3.71174403388056));
#27248=CARTESIAN_POINT('Ctrl Pts',(68.7589309272997,5.96067226948623,-0.994660250423083));
#27249=CARTESIAN_POINT('Ctrl Pts',(69.3115625062471,5.71566070266274,1.96218875872725));
#27250=CARTESIAN_POINT('Ctrl Pts',(69.8641940851944,4.09287504179451,4.44604750227256));
#27251=CARTESIAN_POINT('Ctrl Pts',(70.4168256641419,1.48349122236702,5.85817489580176));
#27252=CARTESIAN_POINT('Ctrl Pts',(70.9694572430892,-1.48349100436534,5.85817564103365));
#27253=CARTESIAN_POINT('Ctrl Pts',(71.5220888220366,-4.09287582201279,4.44604632565119));
#27254=CARTESIAN_POINT('Ctrl Pts',(72.0747204009839,-5.71565890873659,1.96219104782992));
#27255=CARTESIAN_POINT('Ctrl Pts',(72.6273519799313,-5.9606761168237,-0.994664977192599));
#27256=CARTESIAN_POINT('Ctrl Pts',(73.1799835588787,-4.76884068918239,-3.71173413415616));
#27257=CARTESIAN_POINT('Ctrl Pts',(73.732615137826,-2.42749964852484,-5.53412340547436));
#27258=CARTESIAN_POINT('Ctrl Pts',(74.2852467167734,0.499070024096889,-6.02240821551781));
#27259=CARTESIAN_POINT('Ctrl Pts',(74.8378782957208,3.30517718677736,-5.05916675657822));
#27260=CARTESIAN_POINT('Ctrl Pts',(75.3905098746681,5.31486464408031,-2.87600085013837));
#27261=CARTESIAN_POINT('Ctrl Pts',(75.7589309272997,5.79981109503712,-0.958997471436831));
#27262=CARTESIAN_POINT('Ctrl Pts',(75.9431414536155,5.79981109503712,-8.52326411183583E-15));
#27263=CARTESIAN_POINT('Ctrl Pts',(33.62030855087,6.05892730518855,0.));
#27264=CARTESIAN_POINT('Ctrl Pts',(33.8045190771858,6.05892730518855,1.00170122537842));
#27265=CARTESIAN_POINT('Ctrl Pts',(34.1729401298174,5.55226374371841,3.00453419845087));
#27266=CARTESIAN_POINT('Ctrl Pts',(34.7255717087647,3.45282354398353,5.28512205116659));
#27267=CARTESIAN_POINT('Ctrl Pts',(35.2782032877121,0.52135987967838,6.29143885263431));
#27268=CARTESIAN_POINT('Ctrl Pts',(35.8308348666595,-2.53593227701648,5.78132024999939));
#27269=CARTESIAN_POINT('Ctrl Pts',(36.3834664456069,-4.98186108464976,3.87753730806675));
#27270=CARTESIAN_POINT('Ctrl Pts',(36.9360980245542,-6.22693362925883,1.03909408852531));
#27271=CARTESIAN_POINT('Ctrl Pts',(37.4887296035016,-5.97097223597331,-2.04983951271052));
#27272=CARTESIAN_POINT('Ctrl Pts',(38.0413611824489,-4.27570069868504,-4.64464744982032));
#27273=CARTESIAN_POINT('Ctrl Pts',(38.5939927613963,-1.54975720378295,-6.11985471822127));
#27274=CARTESIAN_POINT('Ctrl Pts',(39.1466243403437,1.54975741221459,-6.11985420086809));
#27275=CARTESIAN_POINT('Ctrl Pts',(39.6992559192911,4.27569995271762,-4.64464826665024));
#27276=CARTESIAN_POINT('Ctrl Pts',(40.2518874982384,5.97097395114776,-2.04983792356467));
#27277=CARTESIAN_POINT('Ctrl Pts',(40.8045190771858,6.22692995081589,1.03909080720973));
#27278=CARTESIAN_POINT('Ctrl Pts',(41.3571506561332,4.98186884549998,3.87754418138483));
#27279=CARTESIAN_POINT('Ctrl Pts',(41.9097822350805,2.53591585418045,5.78130580919469));
#27280=CARTESIAN_POINT('Ctrl Pts',(42.4624138140279,-0.521326007358065,
6.29146924994462));
#27281=CARTESIAN_POINT('Ctrl Pts',(43.0150453929753,-3.45290092330605,5.28505830615491));
#27282=CARTESIAN_POINT('Ctrl Pts',(43.5676769719227,-5.55214545226785,3.00467086174248));
#27283=CARTESIAN_POINT('Ctrl Pts',(44.12030855087,-6.31303145085601,-2.06792707167108E-10));
#27284=CARTESIAN_POINT('Ctrl Pts',(44.6729401298174,-5.55214545188636,-3.00467086120918));
#27285=CARTESIAN_POINT('Ctrl Pts',(45.2255717087647,-3.45290092428985,-5.28505830711662));
#27286=CARTESIAN_POINT('Ctrl Pts',(45.7782032877121,-0.521326005202469,
-6.29146924799781));
#27287=CARTESIAN_POINT('Ctrl Pts',(46.3308348666595,2.53591584960525,-5.78130581325357));
#27288=CARTESIAN_POINT('Ctrl Pts',(46.8834664456069,4.98186885514319,-3.87754417286436));
#27289=CARTESIAN_POINT('Ctrl Pts',(47.4360980245542,6.22692993052255,-1.03909082512399));
#27290=CARTESIAN_POINT('Ctrl Pts',(47.9887296035015,5.97097399383832,2.04983796124264));
#27291=CARTESIAN_POINT('Ctrl Pts',(48.541361182449,4.27569986291781,4.64464818739812));
#27292=CARTESIAN_POINT('Ctrl Pts',(49.0939927613963,1.54975760110581,6.11985436757058));
#27293=CARTESIAN_POINT('Ctrl Pts',(49.6466243403437,-1.54975760110596,6.11985436757021));
#27294=CARTESIAN_POINT('Ctrl Pts',(50.199255919291,-4.27569986291726,4.64464818739871));
#27295=CARTESIAN_POINT('Ctrl Pts',(50.7518874982385,-5.97097399383958,2.04983796124148));
#27296=CARTESIAN_POINT('Ctrl Pts',(51.3045190771858,-6.22692993051986,-1.03909082512159));
#27297=CARTESIAN_POINT('Ctrl Pts',(51.8571506561332,-4.98186885514887,-3.87754417286939));
#27298=CARTESIAN_POINT('Ctrl Pts',(52.4097822350806,-2.53591584959328,-5.781305813243));
#27299=CARTESIAN_POINT('Ctrl Pts',(52.9624138140279,0.521326005177292,-6.29146924802002));
#27300=CARTESIAN_POINT('Ctrl Pts',(53.5150453929753,3.45290092434281,-5.28505830706988));
#27301=CARTESIAN_POINT('Ctrl Pts',(54.0676769719227,5.55214545177497,-3.0046708613075));
#27302=CARTESIAN_POINT('Ctrl Pts',(54.62030855087,6.31303145109033,-5.36390383455044E-15));
#27303=CARTESIAN_POINT('Ctrl Pts',(55.1729401298174,5.55214545177497,3.0046708613075));
#27304=CARTESIAN_POINT('Ctrl Pts',(55.7255717087647,3.45290092434281,5.28505830706987));
#27305=CARTESIAN_POINT('Ctrl Pts',(56.2782032877121,0.521326005177289,6.29146924802003));
#27306=CARTESIAN_POINT('Ctrl Pts',(56.8308348666595,-2.5359158495933,5.781305813243));
#27307=CARTESIAN_POINT('Ctrl Pts',(57.3834664456068,-4.98186885514888,3.87754417286939));
#27308=CARTESIAN_POINT('Ctrl Pts',(57.9360980245542,-6.22692993051986,1.03909082512159));
#27309=CARTESIAN_POINT('Ctrl Pts',(58.4887296035016,-5.97097399383958,-2.04983796124148));
#27310=CARTESIAN_POINT('Ctrl Pts',(59.041361182449,-4.27569986291726,-4.64464818739871));
#27311=CARTESIAN_POINT('Ctrl Pts',(59.5939927613963,-1.54975760110596,-6.11985436757021));
#27312=CARTESIAN_POINT('Ctrl Pts',(60.1466243403437,1.5497576011058,-6.11985436757059));
#27313=CARTESIAN_POINT('Ctrl Pts',(60.699255919291,4.2756998629178,-4.64464818739812));
#27314=CARTESIAN_POINT('Ctrl Pts',(61.2518874982385,5.97097399383833,-2.04983796124265));
#27315=CARTESIAN_POINT('Ctrl Pts',(61.8045190771858,6.22692993052255,1.03909082512398));
#27316=CARTESIAN_POINT('Ctrl Pts',(62.3571506561332,4.98186885514319,3.87754417286436));
#27317=CARTESIAN_POINT('Ctrl Pts',(62.9097822350805,2.53591584960525,5.78130581325356));
#27318=CARTESIAN_POINT('Ctrl Pts',(63.4624138140279,-0.521326005202466,
6.2914692479978));
#27319=CARTESIAN_POINT('Ctrl Pts',(64.0150453929752,-3.45290092428985,5.28505830711661));
#27320=CARTESIAN_POINT('Ctrl Pts',(64.5676769719227,-5.55214545188636,3.00467086120919));
#27321=CARTESIAN_POINT('Ctrl Pts',(65.1203085508701,-6.31303145085602,2.06801021218025E-10));
#27322=CARTESIAN_POINT('Ctrl Pts',(65.6729401298174,-5.55214545226785,-3.00467086174248));
#27323=CARTESIAN_POINT('Ctrl Pts',(66.2255717087647,-3.45290092330605,-5.28505830615491));
#27324=CARTESIAN_POINT('Ctrl Pts',(66.7782032877121,-0.521326007358057,
-6.29146924994462));
#27325=CARTESIAN_POINT('Ctrl Pts',(67.3308348666595,2.53591585418046,-5.78130580919469));
#27326=CARTESIAN_POINT('Ctrl Pts',(67.8834664456069,4.98186884549998,-3.87754418138483));
#27327=CARTESIAN_POINT('Ctrl Pts',(68.4360980245542,6.22692995081589,-1.03909080720973));
#27328=CARTESIAN_POINT('Ctrl Pts',(68.9887296035016,5.97097395114776,2.04983792356467));
#27329=CARTESIAN_POINT('Ctrl Pts',(69.541361182449,4.27569995271762,4.64464826665024));
#27330=CARTESIAN_POINT('Ctrl Pts',(70.0939927613963,1.54975741221458,6.1198542008681));
#27331=CARTESIAN_POINT('Ctrl Pts',(70.6466243403438,-1.54975720378297,6.11985471822127));
#27332=CARTESIAN_POINT('Ctrl Pts',(71.199255919291,-4.27570069868505,4.6446474498203));
#27333=CARTESIAN_POINT('Ctrl Pts',(71.7518874982385,-5.9709722359733,2.04983951271053));
#27334=CARTESIAN_POINT('Ctrl Pts',(72.3045190771858,-6.22693362925883,-1.03909408852532));
#27335=CARTESIAN_POINT('Ctrl Pts',(72.8571506561333,-4.98186108464976,-3.87753730806676));
#27336=CARTESIAN_POINT('Ctrl Pts',(73.4097822350805,-2.53593227701648,-5.78132024999937));
#27337=CARTESIAN_POINT('Ctrl Pts',(73.962413814028,0.521359879678368,-6.29143885263431));
#27338=CARTESIAN_POINT('Ctrl Pts',(74.5150453929753,3.45282354398353,-5.2851220511666));
#27339=CARTESIAN_POINT('Ctrl Pts',(75.0676769719227,5.55226374371841,-3.00453419845087));
#27340=CARTESIAN_POINT('Ctrl Pts',(75.4360980245542,6.05892730518855,-1.00170122537842));
#27341=CARTESIAN_POINT('Ctrl Pts',(75.62030855087,6.05892730518855,-8.90405511667878E-15));
#27342=CARTESIAN_POINT('Ctrl Pts',(33.1358237202237,5.94680344913766,0.));
#27343=CARTESIAN_POINT('Ctrl Pts',(33.3200342465395,5.94680344913766,0.983379197578396));
#27344=CARTESIAN_POINT('Ctrl Pts',(33.6884552991711,5.44959421336945,2.94886771297254));
#27345=CARTESIAN_POINT('Ctrl Pts',(34.2410868781184,3.38895443893944,5.18742673184628));
#27346=CARTESIAN_POINT('Ctrl Pts',(34.7937184570658,0.511722382884761,6.17505868653612));
#27347=CARTESIAN_POINT('Ctrl Pts',(35.3463500360132,-2.48903384632581,5.67440885923965));
#27348=CARTESIAN_POINT('Ctrl Pts',(35.8989816149605,-4.88972305399822,3.80581898848347));
#27349=CARTESIAN_POINT('Ctrl Pts',(36.4516131939079,-6.11177024810298,1.01987909450271));
#27350=CARTESIAN_POINT('Ctrl Pts',(37.0042447728553,-5.86054195732468,-2.01192998939814));
#27351=CARTESIAN_POINT('Ctrl Pts',(37.5568763518026,-4.19662395290879,-4.55874653989111));
#27352=CARTESIAN_POINT('Ctrl Pts',(38.10950793075,-1.52109519307483,-6.00667145344936));
#27353=CARTESIAN_POINT('Ctrl Pts',(38.6621395096974,1.5210954270842,-6.00667054754812));
#27354=CARTESIAN_POINT('Ctrl Pts',(39.2147710886447,4.19662311539983,-4.55874797018865));
#27355=CARTESIAN_POINT('Ctrl Pts',(39.7674026675921,5.86054388297712,-2.01192720677863));
#27356=CARTESIAN_POINT('Ctrl Pts',(40.3200342465395,6.11176611825916,1.01987334860882));
#27357=CARTESIAN_POINT('Ctrl Pts',(40.8726658254868,4.88973176722276,3.80583102214387));
#27358=CARTESIAN_POINT('Ctrl Pts',(41.4252974044342,2.4890154081581,5.67438355771667));
#27359=CARTESIAN_POINT('Ctrl Pts',(41.9779289833816,-0.511684353915735,
6.17511179518466));
#27360=CARTESIAN_POINT('Ctrl Pts',(42.5305605623289,-3.38904131388133,5.18731389692575));
#27361=CARTESIAN_POINT('Ctrl Pts',(43.0831921412763,-5.44946140575937,2.9491010349948));
#27362=CARTESIAN_POINT('Ctrl Pts',(43.6358237202237,-6.19627521287463,-3.62104274501345E-10));
#27363=CARTESIAN_POINT('Ctrl Pts',(44.1884552991711,-5.44946140533107,-2.94910103406097));
#27364=CARTESIAN_POINT('Ctrl Pts',(44.7410868781184,-3.38904131498586,-5.18731389860973));
#27365=CARTESIAN_POINT('Ctrl Pts',(45.2937184570658,-0.511684351495615,
-6.17511179177572));
#27366=CARTESIAN_POINT('Ctrl Pts',(45.8463500360132,2.48901540302145,-5.67438356482389));
#27367=CARTESIAN_POINT('Ctrl Pts',(46.3989816149605,4.88973177804935,-3.80583100722426));
#27368=CARTESIAN_POINT('Ctrl Pts',(46.9516131939079,6.11176609547551,-1.01987337997725));
#27369=CARTESIAN_POINT('Ctrl Pts',(47.5042447728553,5.86054393090647,2.01192727275394));
#27370=CARTESIAN_POINT('Ctrl Pts',(48.0568763518026,4.19662301458021,4.55874783141572));
#27371=CARTESIAN_POINT('Ctrl Pts',(48.60950793075,1.52109563915525,6.00667083944942));
#27372=CARTESIAN_POINT('Ctrl Pts',(49.1621395096974,-1.52109563915541,6.00667083944875));
#27373=CARTESIAN_POINT('Ctrl Pts',(49.7147710886447,-4.1966230145796,4.55874783141676));
#27374=CARTESIAN_POINT('Ctrl Pts',(50.2674026675921,-5.86054393090788,2.0119272727519));
#27375=CARTESIAN_POINT('Ctrl Pts',(50.8200342465394,-6.1117660954725,-1.01987337997305));
#27376=CARTESIAN_POINT('Ctrl Pts',(51.3726658254868,-4.88973177805572,-3.80583100723307));
#27377=CARTESIAN_POINT('Ctrl Pts',(51.9252974044342,-2.48901540300802,-5.67438356480538));
#27378=CARTESIAN_POINT('Ctrl Pts',(52.4779289833816,0.511684351467352,-6.17511179181463));
#27379=CARTESIAN_POINT('Ctrl Pts',(53.030560562329,3.38904131504531,-5.18731389852789));
#27380=CARTESIAN_POINT('Ctrl Pts',(53.5831921412763,5.449461405206,-2.94910103423313));
#27381=CARTESIAN_POINT('Ctrl Pts',(54.1358237202237,6.1962752131377,-6.168489409733E-15));
#27382=CARTESIAN_POINT('Ctrl Pts',(54.688455299171,5.44946140520601,2.94910103423312));
#27383=CARTESIAN_POINT('Ctrl Pts',(55.2410868781184,3.38904131504531,5.18731389852788));
#27384=CARTESIAN_POINT('Ctrl Pts',(55.7937184570658,0.511684351467345,6.17511179181463));
#27385=CARTESIAN_POINT('Ctrl Pts',(56.3463500360131,-2.48901540300803,5.67438356480538));
#27386=CARTESIAN_POINT('Ctrl Pts',(56.8989816149606,-4.88973177805573,3.80583100723306));
#27387=CARTESIAN_POINT('Ctrl Pts',(57.4516131939078,-6.1117660954725,1.01987337997304));
#27388=CARTESIAN_POINT('Ctrl Pts',(58.0042447728553,-5.86054393090788,-2.0119272727519));
#27389=CARTESIAN_POINT('Ctrl Pts',(58.5568763518026,-4.1966230145796,-4.55874783141676));
#27390=CARTESIAN_POINT('Ctrl Pts',(59.1095079307501,-1.52109563915542,-6.00667083944875));
#27391=CARTESIAN_POINT('Ctrl Pts',(59.6621395096973,1.52109563915524,-6.00667083944942));
#27392=CARTESIAN_POINT('Ctrl Pts',(60.2147710886447,4.1966230145802,-4.55874783141572));
#27393=CARTESIAN_POINT('Ctrl Pts',(60.7674026675922,5.86054393090647,-2.01192727275395));
#27394=CARTESIAN_POINT('Ctrl Pts',(61.3200342465394,6.11176609547552,1.01987337997724));
#27395=CARTESIAN_POINT('Ctrl Pts',(61.8726658254869,4.88973177804935,3.80583100722426));
#27396=CARTESIAN_POINT('Ctrl Pts',(62.4252974044342,2.48901540302145,5.67438356482389));
#27397=CARTESIAN_POINT('Ctrl Pts',(62.9779289833816,-0.511684351495617,
6.17511179177572));
#27398=CARTESIAN_POINT('Ctrl Pts',(63.5305605623289,-3.38904131498585,5.18731389860973));
#27399=CARTESIAN_POINT('Ctrl Pts',(64.0831921412763,-5.44946140533107,2.94910103406098));
#27400=CARTESIAN_POINT('Ctrl Pts',(64.6358237202237,-6.19627521287463,3.62109504307536E-10));
#27401=CARTESIAN_POINT('Ctrl Pts',(65.188455299171,-5.44946140575937,-2.94910103499479));
#27402=CARTESIAN_POINT('Ctrl Pts',(65.7410868781184,-3.38904131388132,-5.18731389692575));
#27403=CARTESIAN_POINT('Ctrl Pts',(66.2937184570658,-0.511684353915733,
-6.17511179518466));
#27404=CARTESIAN_POINT('Ctrl Pts',(66.8463500360131,2.48901540815811,-5.67438355771667));
#27405=CARTESIAN_POINT('Ctrl Pts',(67.3989816149605,4.88973176722276,-3.80583102214386));
#27406=CARTESIAN_POINT('Ctrl Pts',(67.9516131939078,6.11176611825917,-1.01987334860882));
#27407=CARTESIAN_POINT('Ctrl Pts',(68.5042447728553,5.86054388297712,2.01192720677863));
#27408=CARTESIAN_POINT('Ctrl Pts',(69.0568763518026,4.19662311539983,4.55874797018865));
#27409=CARTESIAN_POINT('Ctrl Pts',(69.60950793075,1.52109542708419,6.00667054754813));
#27410=CARTESIAN_POINT('Ctrl Pts',(70.1621395096974,-1.52109519307484,6.00667145344936));
#27411=CARTESIAN_POINT('Ctrl Pts',(70.7147710886448,-4.19662395290879,4.5587465398911));
#27412=CARTESIAN_POINT('Ctrl Pts',(71.2674026675922,-5.86054195732468,2.01192998939814));
#27413=CARTESIAN_POINT('Ctrl Pts',(71.8200342465394,-6.11177024810298,-1.01987909450272));
#27414=CARTESIAN_POINT('Ctrl Pts',(72.3726658254869,-4.88972305399822,-3.80581898848348));
#27415=CARTESIAN_POINT('Ctrl Pts',(72.9252974044342,-2.48903384632581,-5.67440885923964));
#27416=CARTESIAN_POINT('Ctrl Pts',(73.4779289833816,0.511722382884753,-6.17505868653612));
#27417=CARTESIAN_POINT('Ctrl Pts',(74.0305605623289,3.38895443893944,-5.18742673184629));
#27418=CARTESIAN_POINT('Ctrl Pts',(74.5831921412763,5.44959421336945,-2.94886771297254));
#27419=CARTESIAN_POINT('Ctrl Pts',(74.9516131939079,5.94680344913766,-0.983379197578397));
#27420=CARTESIAN_POINT('Ctrl Pts',(75.1358237202237,5.94680344913766,-8.73928057097385E-15));
#27421=CARTESIAN_POINT('Ctrl Pts',(32.9926516271063,5.64959965017094,0.));
#27422=CARTESIAN_POINT('Ctrl Pts',(33.1768621534221,5.64959965017094,0.934105498328347));
#27423=CARTESIAN_POINT('Ctrl Pts',(33.5452832060536,5.17719316068765,2.80153095913731));
#27424=CARTESIAN_POINT('Ctrl Pts',(34.097914785001,3.21956825042242,4.92810992359527));
#27425=CARTESIAN_POINT('Ctrl Pts',(34.6505463639483,0.486141746602274,5.86641986341936));
#27426=CARTESIAN_POINT('Ctrl Pts',(35.2031779428958,-2.36462122333319,5.39077403004133));
#27427=CARTESIAN_POINT('Ctrl Pts',(35.7558095218431,-4.64531700059631,3.61559300345088));
#27428=CARTESIAN_POINT('Ctrl Pts',(36.3084411007905,-5.80628073241482,0.968900224297807));
#27429=CARTESIAN_POINT('Ctrl Pts',(36.8610726797378,-5.56761023028957,-1.91136547361583));
#27430=CARTESIAN_POINT('Ctrl Pts',(37.4137042586852,-3.98686087342849,-4.33088362081724));
#27431=CARTESIAN_POINT('Ctrl Pts',(37.9663358376326,-1.44506518185627,-5.7064353192738));
#27432=CARTESIAN_POINT('Ctrl Pts',(38.5189674165799,1.445065386745,-5.7064346943363));
#27433=CARTESIAN_POINT('Ctrl Pts',(39.0715989955273,3.98686014014099,-4.33088460750931));
#27434=CARTESIAN_POINT('Ctrl Pts',(39.6242305744747,5.56761191630958,-1.91136355401326));
#27435=CARTESIAN_POINT('Ctrl Pts',(40.1768621534221,5.80627711649786,0.968896260552868));
#27436=CARTESIAN_POINT('Ctrl Pts',(40.7294937323694,4.64532462952802,3.61560130546583));
#27437=CARTESIAN_POINT('Ctrl Pts',(41.2821253113168,2.36460507965162,5.39075658079754));
#27438=CARTESIAN_POINT('Ctrl Pts',(41.8347568902642,-0.486108450041791,
5.86645653965694));
#27439=CARTESIAN_POINT('Ctrl Pts',(42.3873884692115,-3.21964431445548,4.92803248756168));
#27440=CARTESIAN_POINT('Ctrl Pts',(42.9400200481589,-5.17707687994863,2.80169390094401));
#27441=CARTESIAN_POINT('Ctrl Pts',(43.4926516271062,-5.88656213122846,-2.49796196989472E-10));
#27442=CARTESIAN_POINT('Ctrl Pts',(44.0452832060537,-5.17707687957364,-2.80169390029981));
#27443=CARTESIAN_POINT('Ctrl Pts',(44.597914785001,-3.21964431542256,-4.92803248872338));
#27444=CARTESIAN_POINT('Ctrl Pts',(45.1505463639484,-0.486108447922835,
-5.86645653730528));
#27445=CARTESIAN_POINT('Ctrl Pts',(45.7031779428957,2.36460507515419,-5.39075658570046));
#27446=CARTESIAN_POINT('Ctrl Pts',(46.2558095218431,4.64532463900732,-3.61560129517351));
#27447=CARTESIAN_POINT('Ctrl Pts',(46.8084411007904,5.80627709654946,-0.968896282192427));
#27448=CARTESIAN_POINT('Ctrl Pts',(47.3610726797379,5.5676119582745,1.91136359952644));
#27449=CARTESIAN_POINT('Ctrl Pts',(47.9137042586852,3.98686005186758,4.33088451177657));
#27450=CARTESIAN_POINT('Ctrl Pts',(48.4663358376326,1.44506557242546,5.70643489570486));
#27451=CARTESIAN_POINT('Ctrl Pts',(49.0189674165799,-1.4450655724256,5.7064348957044));
#27452=CARTESIAN_POINT('Ctrl Pts',(49.5715989955273,-3.98686005186705,4.3308845117773));
#27453=CARTESIAN_POINT('Ctrl Pts',(50.1242305744747,-5.56761195827573,1.91136359952503));
#27454=CARTESIAN_POINT('Ctrl Pts',(50.6768621534221,-5.80627709654682,-0.968896282189531));
#27455=CARTESIAN_POINT('Ctrl Pts',(51.2294937323694,-4.6453246390129,-3.61560129517959));
#27456=CARTESIAN_POINT('Ctrl Pts',(51.7821253113168,-2.36460507514243,-5.3907565856877));
#27457=CARTESIAN_POINT('Ctrl Pts',(52.3347568902641,0.486108447898087,-5.86645653733213));
#27458=CARTESIAN_POINT('Ctrl Pts',(52.8873884692115,3.21964431547462,-4.92803248866692));
#27459=CARTESIAN_POINT('Ctrl Pts',(53.4400200481589,5.17707687946413,-2.80169390041857));
#27460=CARTESIAN_POINT('Ctrl Pts',(53.9926516271062,5.88656213145879,-3.62063508832155E-15));
#27461=CARTESIAN_POINT('Ctrl Pts',(54.5452832060537,5.17707687946413,2.80169390041857));
#27462=CARTESIAN_POINT('Ctrl Pts',(55.0979147850009,3.21964431547461,4.92803248866692));
#27463=CARTESIAN_POINT('Ctrl Pts',(55.6505463639484,0.486108447898084,5.86645653733212));
#27464=CARTESIAN_POINT('Ctrl Pts',(56.2031779428957,-2.36460507514244,5.3907565856877));
#27465=CARTESIAN_POINT('Ctrl Pts',(56.7558095218431,-4.64532463901291,3.61560129517958));
#27466=CARTESIAN_POINT('Ctrl Pts',(57.3084411007904,-5.80627709654682,0.968896282189525));
#27467=CARTESIAN_POINT('Ctrl Pts',(57.8610726797378,-5.56761195827573,-1.91136359952503));
#27468=CARTESIAN_POINT('Ctrl Pts',(58.4137042586852,-3.98686005186705,-4.3308845117773));
#27469=CARTESIAN_POINT('Ctrl Pts',(58.9663358376325,-1.44506557242561,-5.7064348957044));
#27470=CARTESIAN_POINT('Ctrl Pts',(59.51896741658,1.44506557242545,-5.70643489570486));
#27471=CARTESIAN_POINT('Ctrl Pts',(60.0715989955273,3.98686005186758,-4.33088451177658));
#27472=CARTESIAN_POINT('Ctrl Pts',(60.6242305744747,5.5676119582745,-1.91136359952644));
#27473=CARTESIAN_POINT('Ctrl Pts',(61.176862153422,5.80627709654946,0.968896282192422));
#27474=CARTESIAN_POINT('Ctrl Pts',(61.7294937323694,4.64532463900732,3.61560129517351));
#27475=CARTESIAN_POINT('Ctrl Pts',(62.2821253113167,2.36460507515419,5.39075658570046));
#27476=CARTESIAN_POINT('Ctrl Pts',(62.8347568902642,-0.486108447922834,
5.86645653730528));
#27477=CARTESIAN_POINT('Ctrl Pts',(63.3873884692115,-3.21964431542255,4.92803248872338));
#27478=CARTESIAN_POINT('Ctrl Pts',(63.9400200481589,-5.17707687957363,2.80169390029982));
#27479=CARTESIAN_POINT('Ctrl Pts',(64.4926516271063,-5.88656213122846,2.49803438259616E-10));
#27480=CARTESIAN_POINT('Ctrl Pts',(65.0452832060536,-5.17707687994864,-2.80169390094401));
#27481=CARTESIAN_POINT('Ctrl Pts',(65.597914785001,-3.21964431445548,-4.92803248756169));
#27482=CARTESIAN_POINT('Ctrl Pts',(66.1505463639484,-0.486108450041783,
-5.86645653965694));
#27483=CARTESIAN_POINT('Ctrl Pts',(66.7031779428957,2.36460507965163,-5.39075658079754));
#27484=CARTESIAN_POINT('Ctrl Pts',(67.255809521843,4.64532462952802,-3.61560130546582));
#27485=CARTESIAN_POINT('Ctrl Pts',(67.8084411007905,5.80627711649786,-0.96889626055287));
#27486=CARTESIAN_POINT('Ctrl Pts',(68.3610726797379,5.56761191630958,1.91136355401326));
#27487=CARTESIAN_POINT('Ctrl Pts',(68.9137042586851,3.98686014014099,4.33088460750931));
#27488=CARTESIAN_POINT('Ctrl Pts',(69.4663358376326,1.44506538674499,5.7064346943363));
#27489=CARTESIAN_POINT('Ctrl Pts',(70.0189674165799,-1.44506518185629,5.7064353192738));
#27490=CARTESIAN_POINT('Ctrl Pts',(70.5715989955273,-3.98686087342849,4.33088362081724));
#27491=CARTESIAN_POINT('Ctrl Pts',(71.1242305744747,-5.56761023028957,1.91136547361582));
#27492=CARTESIAN_POINT('Ctrl Pts',(71.6768621534221,-5.80628073241483,-0.968900224297809));
#27493=CARTESIAN_POINT('Ctrl Pts',(72.2294937323694,-4.64531700059631,-3.61559300345089));
#27494=CARTESIAN_POINT('Ctrl Pts',(72.7821253113168,-2.36462122333319,-5.39077403004132));
#27495=CARTESIAN_POINT('Ctrl Pts',(73.3347568902641,0.486141746602262,-5.86641986341937));
#27496=CARTESIAN_POINT('Ctrl Pts',(73.8873884692115,3.21956825042242,-4.92810992359527));
#27497=CARTESIAN_POINT('Ctrl Pts',(74.4400200481589,5.17719316068764,-2.80153095913731));
#27498=CARTESIAN_POINT('Ctrl Pts',(74.8084411007905,5.64959965017094,-0.934105498328348));
#27499=CARTESIAN_POINT('Ctrl Pts',(74.9926516271063,5.64959965017094,-8.30251695365502E-15));
#27500=CARTESIAN_POINT('Ctrl Pts',(32.9926516271063,5.35040034982906,0.));
#27501=CARTESIAN_POINT('Ctrl Pts',(33.1768621534221,5.35040034982906,0.884711999783592));
#27502=CARTESIAN_POINT('Ctrl Pts',(33.5452832060536,4.90303992219514,2.65314027768598));
#27503=CARTESIAN_POINT('Ctrl Pts',(34.097914785001,3.04907159007201,4.66715881783104));
#27504=CARTESIAN_POINT('Ctrl Pts',(34.6505463639483,0.460399720877627,5.55575434845313));
#27505=CARTESIAN_POINT('Ctrl Pts',(35.2031779428958,-2.23940312125801,5.10530860391639));
#27506=CARTESIAN_POINT('Ctrl Pts',(35.7558095218431,-4.39932305117563,3.42412678374845));
#27507=CARTESIAN_POINT('Ctrl Pts',(36.3084411007905,-5.49880832246205,0.917592835722961));
#27508=CARTESIAN_POINT('Ctrl Pts',(36.8610726797378,-5.272776384942,-1.81014920900501));
#27509=CARTESIAN_POINT('Ctrl Pts',(37.4137042586852,-3.77573601188937,-4.10154073270038));
#27510=CARTESIAN_POINT('Ctrl Pts',(37.9663358376326,-1.36854148671349,-5.40425015093622));
#27511=CARTESIAN_POINT('Ctrl Pts',(38.5189674165799,1.36854169117612,-5.40424941809581));
#27512=CARTESIAN_POINT('Ctrl Pts',(39.0715989955273,3.77573528012686,-4.1015418897575));
#27513=CARTESIAN_POINT('Ctrl Pts',(39.6242305744747,5.27277806745566,-1.81014695796662));
#27514=CARTESIAN_POINT('Ctrl Pts',(40.1768621534221,5.49880471406498,0.917588187532836));
#27515=CARTESIAN_POINT('Ctrl Pts',(40.7294937323694,4.39933066424171,3.42413651873231));
#27516=CARTESIAN_POINT('Ctrl Pts',(41.2821253113168,2.23938701114991,5.10528813768847));
#27517=CARTESIAN_POINT('Ctrl Pts',(41.8347568902642,-0.460366493562869,
5.55579732502866));
#27518=CARTESIAN_POINT('Ctrl Pts',(42.3873884692115,-3.04914749591728,4.66706767925751));
#27519=CARTESIAN_POINT('Ctrl Pts',(42.9400200481589,-4.90292388328124,2.65332971861579));
#27520=CARTESIAN_POINT('Ctrl Pts',(43.4926516271062,-5.57483822100387,-2.9292627494233E-10));
#27521=CARTESIAN_POINT('Ctrl Pts',(44.0452832060537,-4.90292388290702,-2.65332971786037));
#27522=CARTESIAN_POINT('Ctrl Pts',(44.597914785001,-3.04914749688235,-4.66706768061979));
#27523=CARTESIAN_POINT('Ctrl Pts',(45.1505463639484,-0.460366491448323,
-5.55579732227095));
#27524=CARTESIAN_POINT('Ctrl Pts',(45.7031779428957,2.23938700666183,-5.10528814343794));
#27525=CARTESIAN_POINT('Ctrl Pts',(46.2558095218431,4.3993306737013,-3.4241365066629));
#27526=CARTESIAN_POINT('Ctrl Pts',(46.8084411007904,5.49880469415807,-0.917588212908723));
#27527=CARTESIAN_POINT('Ctrl Pts',(47.3610726797379,5.2727781093333,1.81014701133818));
#27528=CARTESIAN_POINT('Ctrl Pts',(47.9137042586852,3.77573519203703,4.10154177749537));
#27529=CARTESIAN_POINT('Ctrl Pts',(48.4663358376326,1.36854187647043,5.40424965423309));
#27530=CARTESIAN_POINT('Ctrl Pts',(49.0189674165799,-1.36854187647057,5.40424965423255));
#27531=CARTESIAN_POINT('Ctrl Pts',(49.5715989955273,-3.7757351920365,4.10154177749621));
#27532=CARTESIAN_POINT('Ctrl Pts',(50.1242305744747,-5.27277810933453,1.81014701133654));
#27533=CARTESIAN_POINT('Ctrl Pts',(50.6768621534221,-5.49880469415544,-0.917588212905327));
#27534=CARTESIAN_POINT('Ctrl Pts',(51.2294937323694,-4.39933067370686,-3.42413650667002));
#27535=CARTESIAN_POINT('Ctrl Pts',(51.7821253113168,-2.23938700665009,-5.10528814342298));
#27536=CARTESIAN_POINT('Ctrl Pts',(52.3347568902641,0.460366491423626,-5.55579732230242));
#27537=CARTESIAN_POINT('Ctrl Pts',(52.8873884692115,3.0491474969343,-4.66706768055358));
#27538=CARTESIAN_POINT('Ctrl Pts',(53.4400200481589,4.90292388279774,-2.65332971799963));
#27539=CARTESIAN_POINT('Ctrl Pts',(53.9926516271062,5.57483822123373,-6.57078219732429E-15));
#27540=CARTESIAN_POINT('Ctrl Pts',(54.5452832060537,4.90292388279775,2.65332971799963));
#27541=CARTESIAN_POINT('Ctrl Pts',(55.0979147850009,3.0491474969343,4.66706768055358));
#27542=CARTESIAN_POINT('Ctrl Pts',(55.6505463639484,0.460366491423622,5.55579732230243));
#27543=CARTESIAN_POINT('Ctrl Pts',(56.2031779428957,-2.2393870066501,5.10528814342297));
#27544=CARTESIAN_POINT('Ctrl Pts',(56.7558095218432,-4.39933067370687,3.42413650667002));
#27545=CARTESIAN_POINT('Ctrl Pts',(57.3084411007904,-5.49880469415543,0.917588212905322));
#27546=CARTESIAN_POINT('Ctrl Pts',(57.8610726797378,-5.27277810933453,-1.81014701133654));
#27547=CARTESIAN_POINT('Ctrl Pts',(58.4137042586852,-3.7757351920365,-4.10154177749621));
#27548=CARTESIAN_POINT('Ctrl Pts',(58.9663358376325,-1.36854187647058,-5.40424965423255));
#27549=CARTESIAN_POINT('Ctrl Pts',(59.51896741658,1.36854187647042,-5.40424965423309));
#27550=CARTESIAN_POINT('Ctrl Pts',(60.0715989955273,3.77573519203703,-4.10154177749537));
#27551=CARTESIAN_POINT('Ctrl Pts',(60.6242305744747,5.2727781093333,-1.81014701133819));
#27552=CARTESIAN_POINT('Ctrl Pts',(61.176862153422,5.49880469415808,0.917588212908717));
#27553=CARTESIAN_POINT('Ctrl Pts',(61.7294937323694,4.39933067370129,3.4241365066629));
#27554=CARTESIAN_POINT('Ctrl Pts',(62.2821253113167,2.23938700666183,5.10528814343794));
#27555=CARTESIAN_POINT('Ctrl Pts',(62.8347568902642,-0.460366491448322,
5.55579732227095));
#27556=CARTESIAN_POINT('Ctrl Pts',(63.3873884692115,-3.04914749688234,4.66706768061979));
#27557=CARTESIAN_POINT('Ctrl Pts',(63.9400200481589,-4.90292388290702,2.65332971786038));
#27558=CARTESIAN_POINT('Ctrl Pts',(64.4926516271063,-5.57483822100388,2.92934052602853E-10));
#27559=CARTESIAN_POINT('Ctrl Pts',(65.0452832060536,-4.90292388328124,-2.65332971861579));
#27560=CARTESIAN_POINT('Ctrl Pts',(65.597914785001,-3.04914749591728,-4.66706767925751));
#27561=CARTESIAN_POINT('Ctrl Pts',(66.1505463639483,-0.460366493562863,
-5.55579732502866));
#27562=CARTESIAN_POINT('Ctrl Pts',(66.7031779428957,2.23938701114991,-5.10528813768846));
#27563=CARTESIAN_POINT('Ctrl Pts',(67.2558095218431,4.39933066424171,-3.4241365187323));
#27564=CARTESIAN_POINT('Ctrl Pts',(67.8084411007905,5.49880471406499,-0.917588187532837));
#27565=CARTESIAN_POINT('Ctrl Pts',(68.3610726797379,5.27277806745566,1.81014695796662));
#27566=CARTESIAN_POINT('Ctrl Pts',(68.9137042586851,3.77573528012686,4.1015418897575));
#27567=CARTESIAN_POINT('Ctrl Pts',(69.4663358376326,1.36854169117611,5.40424941809582));
#27568=CARTESIAN_POINT('Ctrl Pts',(70.0189674165799,-1.36854148671351,5.40425015093621));
#27569=CARTESIAN_POINT('Ctrl Pts',(70.5715989955273,-3.77573601188937,4.10154073270038));
#27570=CARTESIAN_POINT('Ctrl Pts',(71.1242305744747,-5.272776384942,1.81014920900501));
#27571=CARTESIAN_POINT('Ctrl Pts',(71.6768621534221,-5.49880832246205,-0.917592835722964));
#27572=CARTESIAN_POINT('Ctrl Pts',(72.2294937323694,-4.39932305117562,-3.42412678374846));
#27573=CARTESIAN_POINT('Ctrl Pts',(72.7821253113168,-2.23940312125801,-5.10530860391638));
#27574=CARTESIAN_POINT('Ctrl Pts',(73.3347568902641,0.460399720877618,-5.55575434845314));
#27575=CARTESIAN_POINT('Ctrl Pts',(73.8873884692115,3.04907159007201,-4.66715881783104));
#27576=CARTESIAN_POINT('Ctrl Pts',(74.4400200481589,4.90303992219514,-2.65314027768598));
#27577=CARTESIAN_POINT('Ctrl Pts',(74.8084411007905,5.35040034982906,-0.884711999783593));
#27578=CARTESIAN_POINT('Ctrl Pts',(74.9926516271063,5.35040034982906,-7.86282079509004E-15));
#27579=CARTESIAN_POINT('Ctrl Pts',(33.1358791011789,5.05215470582044,0.));
#27580=CARTESIAN_POINT('Ctrl Pts',(33.3200896274947,5.05215470582044,0.835439667818526));
#27581=CARTESIAN_POINT('Ctrl Pts',(33.6885106801263,4.62974731329617,2.50523368528442));
#27582=CARTESIAN_POINT('Ctrl Pts',(34.2411422590737,2.87911375329489,4.40702109952745));
#27583=CARTESIAN_POINT('Ctrl Pts',(34.793773838021,0.43473796291613,5.24607120227223));
#27584=CARTESIAN_POINT('Ctrl Pts',(35.3464054169684,-2.11457900308638,4.8207403763615));
#27585=CARTESIAN_POINT('Ctrl Pts',(35.8990369959157,-4.15410404637352,3.23326447896726));
#27586=CARTESIAN_POINT('Ctrl Pts',(36.4516685748631,-5.19230421072891,0.866446616436196));
#27587=CARTESIAN_POINT('Ctrl Pts',(37.0043001538105,-4.9788711625536,-1.70925152427458));
#27588=CARTESIAN_POINT('Ctrl Pts',(37.5569317327579,-3.56527606954637,-3.87292025722597));
#27589=CARTESIAN_POINT('Ctrl Pts',(38.1095633117052,-1.29225881290354,-5.10301667120488));
#27590=CARTESIAN_POINT('Ctrl Pts',(38.6621948906526,1.29225901197644,-5.10301589795954));
#27591=CARTESIAN_POINT('Ctrl Pts',(39.2148264696,3.56527535707347,-3.87292147807751));
#27592=CARTESIAN_POINT('Ctrl Pts',(39.7674580485474,4.97887280071541,-1.70924914912885));
#27593=CARTESIAN_POINT('Ctrl Pts',(40.3200896274947,5.19230069745088,0.8664417119428));
#27594=CARTESIAN_POINT('Ctrl Pts',(40.8727212064421,4.15411145875562,3.23327475046642));
#27595=CARTESIAN_POINT('Ctrl Pts',(41.4253527853894,2.11456331764827,4.82071877979622));
#27596=CARTESIAN_POINT('Ctrl Pts',(41.9779843643368,-0.434705611488933,
5.24611653333821));
#27597=CARTESIAN_POINT('Ctrl Pts',(42.5306159432842,-2.87918765822658,4.40692478140854));
#27598=CARTESIAN_POINT('Ctrl Pts',(43.0832475222315,-4.62963433322232,2.50543281017431));
#27599=CARTESIAN_POINT('Ctrl Pts',(43.6358791011789,-5.26409608723815,-3.09079671340081E-10));
#27600=CARTESIAN_POINT('Ctrl Pts',(44.1885106801263,-4.62963433285796,-2.50543280937723));
#27601=CARTESIAN_POINT('Ctrl Pts',(44.7411422590737,-2.87918765916621,-4.40692478284593));
#27602=CARTESIAN_POINT('Ctrl Pts',(45.293773838021,-0.434705609430123,-5.24611653042846));
#27603=CARTESIAN_POINT('Ctrl Pts',(45.8464054169684,2.1145633132785,-4.82071878586269));
#27604=CARTESIAN_POINT('Ctrl Pts',(46.3990369959157,4.15411146796585,-3.23327473773157));
#27605=CARTESIAN_POINT('Ctrl Pts',(46.9516685748631,5.19230067806873,-0.866441738717781));
#27606=CARTESIAN_POINT('Ctrl Pts',(47.5043001538105,4.97887284148914,1.70924920544305));
#27607=CARTESIAN_POINT('Ctrl Pts',(48.0569317327578,3.56527527130573,3.87292135962583));
#27608=CARTESIAN_POINT('Ctrl Pts',(48.6095633117053,1.2922591923863,5.10301614711619));
#27609=CARTESIAN_POINT('Ctrl Pts',(49.1621948906526,-1.29225919238644,5.10301614711562));
#27610=CARTESIAN_POINT('Ctrl Pts',(49.7148264696,-3.56527527130521,3.87292135962672));
#27611=CARTESIAN_POINT('Ctrl Pts',(50.2674580485474,-4.97887284149034,1.70924920544131));
#27612=CARTESIAN_POINT('Ctrl Pts',(50.8200896274947,-5.19230067806616,-0.866441738714198));
#27613=CARTESIAN_POINT('Ctrl Pts',(51.3727212064421,-4.15411146797128,-3.23327473773908));
#27614=CARTESIAN_POINT('Ctrl Pts',(51.9253527853894,-2.11456331326706,-4.8207187858469));
#27615=CARTESIAN_POINT('Ctrl Pts',(52.4779843643368,0.434705609406076,-5.24611653046166));
#27616=CARTESIAN_POINT('Ctrl Pts',(53.0306159432842,2.87918765921679,-4.40692478277608));
#27617=CARTESIAN_POINT('Ctrl Pts',(53.5832475222316,4.62963433275156,-2.50543280952418));
#27618=CARTESIAN_POINT('Ctrl Pts',(54.1358791011789,5.26409608746195,-1.74326874622889E-15));
#27619=CARTESIAN_POINT('Ctrl Pts',(54.6885106801263,4.62963433275157,2.50543280952417));
#27620=CARTESIAN_POINT('Ctrl Pts',(55.2411422590736,2.87918765921679,4.40692478277608));
#27621=CARTESIAN_POINT('Ctrl Pts',(55.793773838021,0.434705609406073,5.24611653046167));
#27622=CARTESIAN_POINT('Ctrl Pts',(56.3464054169684,-2.11456331326707,4.82071878584689));
#27623=CARTESIAN_POINT('Ctrl Pts',(56.8990369959158,-4.15411146797128,3.23327473773908));
#27624=CARTESIAN_POINT('Ctrl Pts',(57.4516685748631,-5.19230067806616,0.866441738714194));
#27625=CARTESIAN_POINT('Ctrl Pts',(58.0043001538105,-4.97887284149034,-1.70924920544131));
#27626=CARTESIAN_POINT('Ctrl Pts',(58.5569317327579,-3.56527527130521,-3.87292135962672));
#27627=CARTESIAN_POINT('Ctrl Pts',(59.1095633117052,-1.29225919238644,-5.10301614711562));
#27628=CARTESIAN_POINT('Ctrl Pts',(59.6621948906526,1.29225919238629,-5.10301614711619));
#27629=CARTESIAN_POINT('Ctrl Pts',(60.2148264696,3.56527527130572,-3.87292135962584));
#27630=CARTESIAN_POINT('Ctrl Pts',(60.7674580485473,4.97887284148913,-1.70924920544305));
#27631=CARTESIAN_POINT('Ctrl Pts',(61.3200896274947,5.19230067806873,0.866441738717778));
#27632=CARTESIAN_POINT('Ctrl Pts',(61.8727212064421,4.15411146796585,3.23327473773157));
#27633=CARTESIAN_POINT('Ctrl Pts',(62.4253527853894,2.11456331327849,4.82071878586269));
#27634=CARTESIAN_POINT('Ctrl Pts',(62.9779843643369,-0.434705609430122,
5.24611653042845));
#27635=CARTESIAN_POINT('Ctrl Pts',(63.5306159432841,-2.8791876591662,4.40692478284593));
#27636=CARTESIAN_POINT('Ctrl Pts',(64.0832475222316,-4.62963433285796,2.50543280937724));
#27637=CARTESIAN_POINT('Ctrl Pts',(64.6358791011789,-5.26409608723815,3.09085705731855E-10));
#27638=CARTESIAN_POINT('Ctrl Pts',(65.1885106801263,-4.62963433322232,-2.50543281017431));
#27639=CARTESIAN_POINT('Ctrl Pts',(65.7411422590737,-2.87918765822658,-4.40692478140855));
#27640=CARTESIAN_POINT('Ctrl Pts',(66.293773838021,-0.434705611488927,-5.24611653333821));
#27641=CARTESIAN_POINT('Ctrl Pts',(66.8464054169685,2.11456331764827,-4.82071877979622));
#27642=CARTESIAN_POINT('Ctrl Pts',(67.3990369959157,4.15411145875562,-3.23327475046641));
#27643=CARTESIAN_POINT('Ctrl Pts',(67.9516685748631,5.19230069745088,-0.866441711942802));
#27644=CARTESIAN_POINT('Ctrl Pts',(68.5043001538105,4.97887280071541,1.70924914912885));
#27645=CARTESIAN_POINT('Ctrl Pts',(69.0569317327578,3.56527535707346,3.87292147807751));
#27646=CARTESIAN_POINT('Ctrl Pts',(69.6095633117052,1.29225901197643,5.10301589795954));
#27647=CARTESIAN_POINT('Ctrl Pts',(70.1621948906526,-1.29225881290355,5.10301667120488));
#27648=CARTESIAN_POINT('Ctrl Pts',(70.7148264696,-3.56527606954638,3.87292025722596));
#27649=CARTESIAN_POINT('Ctrl Pts',(71.2674580485474,-4.9788711625536,1.70925152427458));
#27650=CARTESIAN_POINT('Ctrl Pts',(71.8200896274948,-5.19230421072891,-0.866446616436202));
#27651=CARTESIAN_POINT('Ctrl Pts',(72.3727212064421,-4.15410404637352,-3.23326447896727));
#27652=CARTESIAN_POINT('Ctrl Pts',(72.9253527853895,-2.11457900308638,-4.82074037636149));
#27653=CARTESIAN_POINT('Ctrl Pts',(73.4779843643368,0.434737962916119,-5.24607120227223));
#27654=CARTESIAN_POINT('Ctrl Pts',(74.0306159432842,2.87911375329489,-4.40702109952745));
#27655=CARTESIAN_POINT('Ctrl Pts',(74.5832475222315,4.62974731329617,-2.50523368528442));
#27656=CARTESIAN_POINT('Ctrl Pts',(74.9516685748631,5.05215470582044,-0.835439667818527));
#27657=CARTESIAN_POINT('Ctrl Pts',(75.1358791011789,5.05215470582044,-7.4245261071363E-15));
#27658=CARTESIAN_POINT('Ctrl Pts',(33.6197755720781,4.94250112032697,0.));
#27659=CARTESIAN_POINT('Ctrl Pts',(33.8039860983939,4.94250112032697,0.817139076837683));
#27660=CARTESIAN_POINT('Ctrl Pts',(34.1724071510254,4.52920068974087,2.45091075495199));
#27661=CARTESIAN_POINT('Ctrl Pts',(34.7250387299729,2.81660319447189,4.31128469373266));
#27662=CARTESIAN_POINT('Ctrl Pts',(35.2776703089202,0.42529402211631,5.13217251323705));
#27663=CARTESIAN_POINT('Ctrl Pts',(35.8303018878676,-2.06865974125642,4.71605075332317));
#27664=CARTESIAN_POINT('Ctrl Pts',(36.3829334668149,-4.06389977762583,3.16305923338873));
#27665=CARTESIAN_POINT('Ctrl Pts',(36.9355650457623,-5.07955447125059,0.847630025952494));
#27666=CARTESIAN_POINT('Ctrl Pts',(37.4881966247097,-4.87075665964084,-1.67213470664358));
#27667=CARTESIAN_POINT('Ctrl Pts',(38.0408282036571,-3.48785707483957,-3.78882139657513));
#27668=CARTESIAN_POINT('Ctrl Pts',(38.5934597826044,-1.26419784346094,-4.9922059811041));
#27669=CARTESIAN_POINT('Ctrl Pts',(39.1460913615518,1.26419801522272,-4.99220553559825));
#27670=CARTESIAN_POINT('Ctrl Pts',(39.6987229404992,3.48785646011191,-3.78882209996813));
#27671=CARTESIAN_POINT('Ctrl Pts',(40.2513545194465,4.87075807306072,-1.67213333819149));
#27672=CARTESIAN_POINT('Ctrl Pts',(40.8039860983939,5.07955143996455,0.847627200316705));
#27673=CARTESIAN_POINT('Ctrl Pts',(41.3566176773413,4.06390617309189,3.16306515207384));
#27674=CARTESIAN_POINT('Ctrl Pts',(41.9092492562886,2.06864620772757,4.71603831708452));
#27675=CARTESIAN_POINT('Ctrl Pts',(42.461880835236,-0.425266109030922,5.13219868216793));
#27676=CARTESIAN_POINT('Ctrl Pts',(43.0145124141834,-2.81666696027288,4.3112297296128));
#27677=CARTESIAN_POINT('Ctrl Pts',(43.5671439931307,-4.52910320957627,2.45102808648086));
#27678=CARTESIAN_POINT('Ctrl Pts',(44.1197755720781,-5.14978781662001,-1.78074231939325E-10));
#27679=CARTESIAN_POINT('Ctrl Pts',(44.6724071510254,-4.5291032092619,-2.45102808602162));
#27680=CARTESIAN_POINT('Ctrl Pts',(45.2250387299728,-2.8166669610836,-4.31122973044095));
#27681=CARTESIAN_POINT('Ctrl Pts',(45.7776703089202,-0.425266107254567,
-5.13219868049148));
#27682=CARTESIAN_POINT('Ctrl Pts',(46.3303018878675,2.06864620395729,-4.71603832057972));
#27683=CARTESIAN_POINT('Ctrl Pts',(46.882933466815,4.06390618103855,-3.16306514473666));
#27684=CARTESIAN_POINT('Ctrl Pts',(47.4355650457623,5.07955142324146,-0.847627215743122));
#27685=CARTESIAN_POINT('Ctrl Pts',(47.9881966247097,4.87075810824064,1.67213337063694));
#27686=CARTESIAN_POINT('Ctrl Pts',(48.540828203657,3.48785638611078,3.78882203172213));
#27687=CARTESIAN_POINT('Ctrl Pts',(49.0934597826044,1.26419817088188,4.99220567914997));
#27688=CARTESIAN_POINT('Ctrl Pts',(49.6460913615518,-1.264198170882,4.99220567914965));
#27689=CARTESIAN_POINT('Ctrl Pts',(50.1987229404991,-3.48785638611033,3.78882203172264));
#27690=CARTESIAN_POINT('Ctrl Pts',(50.7513545194465,-4.87075810824168,1.67213337063594));
#27691=CARTESIAN_POINT('Ctrl Pts',(51.3039860983939,-5.07955142323925,-0.847627215741061));
#27692=CARTESIAN_POINT('Ctrl Pts',(51.8566176773412,-4.06390618104323,-3.16306514474098));
#27693=CARTESIAN_POINT('Ctrl Pts',(52.4092492562886,-2.06864620394743,-4.71603832057063));
#27694=CARTESIAN_POINT('Ctrl Pts',(52.961880835236,0.425266107233821,-5.13219868051061));
#27695=CARTESIAN_POINT('Ctrl Pts',(53.5145124141833,2.81666696112724,-4.31122973040071));
#27696=CARTESIAN_POINT('Ctrl Pts',(54.0671439931307,4.5291032091701,-2.45102808610628));
#27697=CARTESIAN_POINT('Ctrl Pts',(54.6197755720781,5.14978781681311,-5.90029421800548E-15));
#27698=CARTESIAN_POINT('Ctrl Pts',(55.1724071510255,4.52910320917011,2.45102808610628));
#27699=CARTESIAN_POINT('Ctrl Pts',(55.7250387299728,2.81666696112724,4.3112297304007));
#27700=CARTESIAN_POINT('Ctrl Pts',(56.2776703089202,0.425266107233817,5.13219868051062));
#27701=CARTESIAN_POINT('Ctrl Pts',(56.8303018878676,-2.06864620394744,4.71603832057062));
#27702=CARTESIAN_POINT('Ctrl Pts',(57.3829334668149,-4.06390618104323,3.16306514474098));
#27703=CARTESIAN_POINT('Ctrl Pts',(57.9355650457622,-5.07955142323925,0.847627215741054));
#27704=CARTESIAN_POINT('Ctrl Pts',(58.4881966247097,-4.87075810824168,-1.67213337063594));
#27705=CARTESIAN_POINT('Ctrl Pts',(59.0408282036571,-3.48785638611033,-3.78882203172264));
#27706=CARTESIAN_POINT('Ctrl Pts',(59.5934597826044,-1.26419817088201,-4.99220567914965));
#27707=CARTESIAN_POINT('Ctrl Pts',(60.1460913615518,1.26419817088187,-4.99220567914997));
#27708=CARTESIAN_POINT('Ctrl Pts',(60.6987229404992,3.48785638611077,-3.78882203172213));
#27709=CARTESIAN_POINT('Ctrl Pts',(61.2513545194465,4.87075810824064,-1.67213337063695));
#27710=CARTESIAN_POINT('Ctrl Pts',(61.8039860983939,5.07955142324146,0.847627215743118));
#27711=CARTESIAN_POINT('Ctrl Pts',(62.3566176773412,4.06390618103855,3.16306514473665));
#27712=CARTESIAN_POINT('Ctrl Pts',(62.9092492562886,2.06864620395729,4.71603832057972));
#27713=CARTESIAN_POINT('Ctrl Pts',(63.461880835236,-0.425266107254564,5.13219868049148));
#27714=CARTESIAN_POINT('Ctrl Pts',(64.0145124141834,-2.8166669610836,4.31122973044095));
#27715=CARTESIAN_POINT('Ctrl Pts',(64.5671439931307,-4.5291032092619,2.45102808602162));
#27716=CARTESIAN_POINT('Ctrl Pts',(65.1197755720782,-5.14978781662001,1.78081473209479E-10));
#27717=CARTESIAN_POINT('Ctrl Pts',(65.6724071510254,-4.52910320957627,-2.45102808648086));
#27718=CARTESIAN_POINT('Ctrl Pts',(66.2250387299728,-2.81666696027288,-4.3112297296128));
#27719=CARTESIAN_POINT('Ctrl Pts',(66.7776703089202,-0.425266109030917,
-5.13219868216794));
#27720=CARTESIAN_POINT('Ctrl Pts',(67.3303018878675,2.06864620772757,-4.71603831708452));
#27721=CARTESIAN_POINT('Ctrl Pts',(67.8829334668149,4.06390617309189,-3.16306515207384));
#27722=CARTESIAN_POINT('Ctrl Pts',(68.4355650457623,5.07955143996455,-0.847627200316705));
#27723=CARTESIAN_POINT('Ctrl Pts',(68.9881966247097,4.87075807306072,1.67213333819149));
#27724=CARTESIAN_POINT('Ctrl Pts',(69.540828203657,3.48785646011191,3.78882209996812));
#27725=CARTESIAN_POINT('Ctrl Pts',(70.0934597826044,1.26419801522272,4.99220553559826));
#27726=CARTESIAN_POINT('Ctrl Pts',(70.6460913615518,-1.26419784346096,4.99220598110409));
#27727=CARTESIAN_POINT('Ctrl Pts',(71.1987229404992,-3.48785707483957,3.78882139657512));
#27728=CARTESIAN_POINT('Ctrl Pts',(71.7513545194465,-4.87075665964084,1.67213470664358));
#27729=CARTESIAN_POINT('Ctrl Pts',(72.3039860983939,-5.0795544712506,-0.847630025952498));
#27730=CARTESIAN_POINT('Ctrl Pts',(72.8566176773413,-4.06389977762583,-3.16305923338874));
#27731=CARTESIAN_POINT('Ctrl Pts',(73.4092492562886,-2.06865974125642,-4.71605075332316));
#27732=CARTESIAN_POINT('Ctrl Pts',(73.961880835236,0.425294022116303,-5.13217251323706));
#27733=CARTESIAN_POINT('Ctrl Pts',(74.5145124141834,2.81660319447188,-4.31128469373267));
#27734=CARTESIAN_POINT('Ctrl Pts',(75.0671439931307,4.52920068974087,-2.45091075495198));
#27735=CARTESIAN_POINT('Ctrl Pts',(75.4355650457623,4.94250112032697,-0.817139076837684));
#27736=CARTESIAN_POINT('Ctrl Pts',(75.6197755720781,4.94250112032697,-7.26338181214876E-15));
#27737=CARTESIAN_POINT('Ctrl Pts',(33.9441734627902,5.19996900808372,0.));
#27738=CARTESIAN_POINT('Ctrl Pts',(34.128383989106,5.19996900808372,0.859814026526804));
#27739=CARTESIAN_POINT('Ctrl Pts',(34.4968050417376,4.76517797451894,2.57855204094631));
#27740=CARTESIAN_POINT('Ctrl Pts',(35.0494366206849,2.96334119934827,4.53592553639668));
#27741=CARTESIAN_POINT('Ctrl Pts',(35.6020681996323,0.447454012565768,5.39954421798947));
#27742=CARTESIAN_POINT('Ctrl Pts',(36.1546997785797,-2.17643695412734,4.96176002173633));
#27743=CARTESIAN_POINT('Ctrl Pts',(36.707331357527,-4.27562619453865,3.32785024601096));
#27744=CARTESIAN_POINT('Ctrl Pts',(37.2599629364744,-5.34419675899476,0.891792351082074));
#27745=CARTESIAN_POINT('Ctrl Pts',(37.8125945154218,-5.12452030784397,-1.75925261524249));
#27746=CARTESIAN_POINT('Ctrl Pts',(38.3652260943691,-3.66957259079425,-3.98621664555567));
#27747=CARTESIAN_POINT('Ctrl Pts',(38.9178576733165,-1.33006183535942,-5.25229733317933));
#27748=CARTESIAN_POINT('Ctrl Pts',(39.4704892522639,1.33006203085693,-5.25229666444782));
#27749=CARTESIAN_POINT('Ctrl Pts',(40.0231208312112,3.6695718911175,-3.98621770139316));
#27750=CARTESIAN_POINT('Ctrl Pts',(40.5757524101586,5.12452191658404,-1.75925056112342));
#27751=CARTESIAN_POINT('Ctrl Pts',(41.1283839891059,5.34419330881595,0.891788109530082));
#27752=CARTESIAN_POINT('Ctrl Pts',(41.6810155680534,4.27563347379279,3.32785912949593));
#27753=CARTESIAN_POINT('Ctrl Pts',(42.2336471470007,2.17642155040303,4.96174134693238));
#27754=CARTESIAN_POINT('Ctrl Pts',(42.7862787259481,-0.44742224217709,5.39958344300911));
#27755=CARTESIAN_POINT('Ctrl Pts',(43.3389103048954,-2.96341377693166,4.53584245342762));
#27756=CARTESIAN_POINT('Ctrl Pts',(43.8915418838428,-4.76506702359125,2.57872531691644));
#27757=CARTESIAN_POINT('Ctrl Pts',(44.4441734627902,-5.41808896103925,-2.67301766495115E-10));
#27758=CARTESIAN_POINT('Ctrl Pts',(44.9968050417375,-4.76506702323344,-2.5787253162271));
#27759=CARTESIAN_POINT('Ctrl Pts',(45.5494366206849,-2.96341377785441,-4.53584245467072));
#27760=CARTESIAN_POINT('Ctrl Pts',(46.1020681996323,-0.447422240155257,
-5.39958344049266));
#27761=CARTESIAN_POINT('Ctrl Pts',(46.6546997785796,2.17642154611174,-4.96174135217889));
#27762=CARTESIAN_POINT('Ctrl Pts',(47.207331357527,4.27563348283759,-3.32785911848237));
#27763=CARTESIAN_POINT('Ctrl Pts',(47.7599629364744,5.3441932897819,-0.891788132686083));
#27764=CARTESIAN_POINT('Ctrl Pts',(48.3125945154218,5.12452195662546,1.75925060982603));
#27765=CARTESIAN_POINT('Ctrl Pts',(48.8652260943691,3.66957180689017,3.98621759895172));
#27766=CARTESIAN_POINT('Ctrl Pts',(49.4178576733165,1.33006220802659,5.25229687992779));
#27767=CARTESIAN_POINT('Ctrl Pts',(49.9704892522639,-1.33006220802673,5.2522968799273));
#27768=CARTESIAN_POINT('Ctrl Pts',(50.5231208312112,-3.66957180688966,3.9862175989525));
#27769=CARTESIAN_POINT('Ctrl Pts',(51.0757524101586,-5.12452195662665,1.75925060982452));
#27770=CARTESIAN_POINT('Ctrl Pts',(51.628383989106,-5.34419328977938,-0.891788132682984));
#27771=CARTESIAN_POINT('Ctrl Pts',(52.1810155680533,-4.27563348284292,-3.32785911848886));
#27772=CARTESIAN_POINT('Ctrl Pts',(52.7336471470007,-2.17642154610051,-4.96174135216523));
#27773=CARTESIAN_POINT('Ctrl Pts',(53.2862787259481,0.447422240131642,-5.39958344052137));
#27774=CARTESIAN_POINT('Ctrl Pts',(53.8389103048955,2.96341377790408,-4.53584245461031));
#27775=CARTESIAN_POINT('Ctrl Pts',(54.3915418838428,4.76506702312895,-2.57872531635419));
#27776=CARTESIAN_POINT('Ctrl Pts',(54.9441734627902,5.41808896125903,-4.00057827660221E-15));
#27777=CARTESIAN_POINT('Ctrl Pts',(55.4968050417376,4.76506702312896,2.57872531635418));
#27778=CARTESIAN_POINT('Ctrl Pts',(56.0494366206849,2.96341377790408,4.5358424546103));
#27779=CARTESIAN_POINT('Ctrl Pts',(56.6020681996323,0.44742224013164,5.39958344052138));
#27780=CARTESIAN_POINT('Ctrl Pts',(57.1546997785797,-2.17642154610052,4.96174135216522));
#27781=CARTESIAN_POINT('Ctrl Pts',(57.707331357527,-4.27563348284293,3.32785911848886));
#27782=CARTESIAN_POINT('Ctrl Pts',(58.2599629364744,-5.34419328977938,0.89178813268298));
#27783=CARTESIAN_POINT('Ctrl Pts',(58.8125945154218,-5.12452195662665,-1.75925060982453));
#27784=CARTESIAN_POINT('Ctrl Pts',(59.3652260943691,-3.66957180688966,-3.9862175989525));
#27785=CARTESIAN_POINT('Ctrl Pts',(59.9178576733165,-1.33006220802674,-5.2522968799273));
#27786=CARTESIAN_POINT('Ctrl Pts',(60.4704892522639,1.33006220802658,-5.2522968799278));
#27787=CARTESIAN_POINT('Ctrl Pts',(61.0231208312112,3.66957180689017,-3.98621759895173));
#27788=CARTESIAN_POINT('Ctrl Pts',(61.5757524101587,5.12452195662546,-1.75925060982604));
#27789=CARTESIAN_POINT('Ctrl Pts',(62.128383989106,5.3441932897819,0.891788132686079));
#27790=CARTESIAN_POINT('Ctrl Pts',(62.6810155680533,4.27563348283759,3.32785911848237));
#27791=CARTESIAN_POINT('Ctrl Pts',(63.2336471470007,2.17642154611174,4.96174135217889));
#27792=CARTESIAN_POINT('Ctrl Pts',(63.7862787259481,-0.447422240155256,
5.39958344049265));
#27793=CARTESIAN_POINT('Ctrl Pts',(64.3389103048954,-2.96341377785441,4.53584245467072));
#27794=CARTESIAN_POINT('Ctrl Pts',(64.8915418838428,-4.76506702323344,2.57872531622711));
#27795=CARTESIAN_POINT('Ctrl Pts',(65.4441734627902,-5.41808896103925,2.67308784269264E-10));
#27796=CARTESIAN_POINT('Ctrl Pts',(65.9968050417376,-4.76506702359125,-2.57872531691644));
#27797=CARTESIAN_POINT('Ctrl Pts',(66.5494366206849,-2.96341377693166,-4.53584245342762));
#27798=CARTESIAN_POINT('Ctrl Pts',(67.1020681996323,-0.447422242177083,
-5.39958344300911));
#27799=CARTESIAN_POINT('Ctrl Pts',(67.6546997785796,2.17642155040303,-4.96174134693238));
#27800=CARTESIAN_POINT('Ctrl Pts',(68.2073313575271,4.27563347379279,-3.32785912949593));
#27801=CARTESIAN_POINT('Ctrl Pts',(68.7599629364744,5.34419330881595,-0.891788109530083));
#27802=CARTESIAN_POINT('Ctrl Pts',(69.3125945154218,5.12452191658404,1.75925056112342));
#27803=CARTESIAN_POINT('Ctrl Pts',(69.8652260943691,3.6695718911175,3.98621770139316));
#27804=CARTESIAN_POINT('Ctrl Pts',(70.4178576733165,1.33006203085692,5.25229666444782));
#27805=CARTESIAN_POINT('Ctrl Pts',(70.9704892522639,-1.33006183535944,5.25229733317932));
#27806=CARTESIAN_POINT('Ctrl Pts',(71.5231208312112,-3.66957259079425,3.98621664555566));
#27807=CARTESIAN_POINT('Ctrl Pts',(72.0757524101586,-5.12452030784397,1.75925261524249));
#27808=CARTESIAN_POINT('Ctrl Pts',(72.628383989106,-5.34419675899477,-0.891792351082077));
#27809=CARTESIAN_POINT('Ctrl Pts',(73.1810155680534,-4.27562619453864,-3.32785024601098));
#27810=CARTESIAN_POINT('Ctrl Pts',(73.7336471470007,-2.17643695412734,-4.96176002173632));
#27811=CARTESIAN_POINT('Ctrl Pts',(74.2862787259481,0.447454012565758,-5.39954421798947));
#27812=CARTESIAN_POINT('Ctrl Pts',(74.8389103048955,2.96334119934827,-4.53592553639669));
#27813=CARTESIAN_POINT('Ctrl Pts',(75.3915418838428,4.76517797451894,-2.5785520409463));
#27814=CARTESIAN_POINT('Ctrl Pts',(75.7599629364744,5.19996900808372,-0.859814026526805));
#27815=CARTESIAN_POINT('Ctrl Pts',(75.9441734627902,5.19996900808372,-7.6417504816982E-15));
#27816=CARTESIAN_POINT('Ctrl Pts',(33.992328768859,5.42478616651165,0.));
#27817=CARTESIAN_POINT('Ctrl Pts',(34.1765392951748,5.42478616651165,0.897005658049128));
#27818=CARTESIAN_POINT('Ctrl Pts',(34.5449603478064,4.97120383948995,2.69002843971947));
#27819=CARTESIAN_POINT('Ctrl Pts',(35.0975919267537,3.09146156820945,4.73204241007042));
#27820=CARTESIAN_POINT('Ctrl Pts',(35.6502235057011,0.46680027700504,5.63299379713529));
#27821=CARTESIAN_POINT('Ctrl Pts',(36.2028550846485,-2.27053630835485,5.1762847224297));
#27822=CARTESIAN_POINT('Ctrl Pts',(36.7554866635958,-4.46048458163846,3.47173079196878));
#27823=CARTESIAN_POINT('Ctrl Pts',(37.3081182425432,-5.57525537632878,0.930349576908284));
#27824=CARTESIAN_POINT('Ctrl Pts',(37.8607498214906,-5.34608105725119,-1.83531473574165));
#27825=CARTESIAN_POINT('Ctrl Pts',(38.4133814004379,-3.82822810044738,-4.15856233495235));
#27826=CARTESIAN_POINT('Ctrl Pts',(38.9660129793853,-1.3875676081727,-5.47938261924127));
#27827=CARTESIAN_POINT('Ctrl Pts',(39.5186445583327,1.38756781460722,-5.47938188798928));
#27828=CARTESIAN_POINT('Ctrl Pts',(40.07127613728,3.82822736162757,-4.1585634895015));
#27829=CARTESIAN_POINT('Ctrl Pts',(40.6239077162274,5.34608275599143,-1.83531248958194));
#27830=CARTESIAN_POINT('Ctrl Pts',(41.1765392951747,5.57525173313143,0.93034493879696));
#27831=CARTESIAN_POINT('Ctrl Pts',(41.7291708741222,4.46049226812687,3.471740505884));
#27832=CARTESIAN_POINT('Ctrl Pts',(42.2818024530695,2.27052004287681,5.17626430084314));
#27833=CARTESIAN_POINT('Ctrl Pts',(42.8344340320169,-0.466766729237704,
5.6330366827348));
#27834=CARTESIAN_POINT('Ctrl Pts',(43.3870656109642,-3.09153820610978,4.73195149145368));
#27835=CARTESIAN_POINT('Ctrl Pts',(43.9396971899116,-4.97108668146758,2.69021758030695));
#27836=CARTESIAN_POINT('Ctrl Pts',(44.492328768859,-5.65234229441848,-2.92291792167501E-10));
#27837=CARTESIAN_POINT('Ctrl Pts',(45.0449603478063,-4.97108668108975,-2.69021757955316));
#27838=CARTESIAN_POINT('Ctrl Pts',(45.5975919267537,-3.09153820708416,-4.731951492813));
#27839=CARTESIAN_POINT('Ctrl Pts',(46.1502235057011,-0.466766727102762,
-5.63303667998308));
#27840=CARTESIAN_POINT('Ctrl Pts',(46.7028550846484,2.27052003834545,-5.17626430658015));
#27841=CARTESIAN_POINT('Ctrl Pts',(47.2554866635958,4.46049227767768,-3.47174049384076));
#27842=CARTESIAN_POINT('Ctrl Pts',(47.8081182425432,5.57525171303253,-0.930344964117844));
#27843=CARTESIAN_POINT('Ctrl Pts',(48.3607498214906,5.34608279827294,1.83531254283782));
#27844=CARTESIAN_POINT('Ctrl Pts',(48.9133814004379,3.82822727268818,4.15856337748268));
#27845=CARTESIAN_POINT('Ctrl Pts',(49.4660129793853,1.38756800168855,5.47938212361473));
#27846=CARTESIAN_POINT('Ctrl Pts',(50.0186445583327,-1.3875680016887,5.4793821236142));
#27847=CARTESIAN_POINT('Ctrl Pts',(50.57127613728,-3.82822727268764,4.15856337748353));
#27848=CARTESIAN_POINT('Ctrl Pts',(51.1239077162274,-5.34608279827419,1.83531254283617));
#27849=CARTESIAN_POINT('Ctrl Pts',(51.6765392951748,-5.57525171302987,-0.930344964114455));
#27850=CARTESIAN_POINT('Ctrl Pts',(52.2291708741221,-4.46049227768331,-3.47174049384787));
#27851=CARTESIAN_POINT('Ctrl Pts',(52.7818024530695,-2.27052003833359,-5.17626430656522));
#27852=CARTESIAN_POINT('Ctrl Pts',(53.3344340320169,0.466766727077827,-5.63303668001448));
#27853=CARTESIAN_POINT('Ctrl Pts',(53.8870656109643,3.09153820713661,-4.73195149274695));
#27854=CARTESIAN_POINT('Ctrl Pts',(54.4396971899116,4.97108668097941,-2.69021757969212));
#27855=CARTESIAN_POINT('Ctrl Pts',(54.992328768859,5.65234229465055,-4.82192605126774E-15));
#27856=CARTESIAN_POINT('Ctrl Pts',(55.5449603478064,4.97108668097942,2.69021757969212));
#27857=CARTESIAN_POINT('Ctrl Pts',(56.0975919267537,3.09153820713661,4.73195149274694));
#27858=CARTESIAN_POINT('Ctrl Pts',(56.6502235057011,0.466766727077823,5.63303668001448));
#27859=CARTESIAN_POINT('Ctrl Pts',(57.2028550846485,-2.2705200383336,5.17626430656521));
#27860=CARTESIAN_POINT('Ctrl Pts',(57.7554866635958,-4.46049227768332,3.47174049384786));
#27861=CARTESIAN_POINT('Ctrl Pts',(58.3081182425432,-5.57525171302987,0.930344964114451));
#27862=CARTESIAN_POINT('Ctrl Pts',(58.8607498214906,-5.34608279827419,-1.83531254283618));
#27863=CARTESIAN_POINT('Ctrl Pts',(59.4133814004379,-3.82822727268764,-4.15856337748353));
#27864=CARTESIAN_POINT('Ctrl Pts',(59.9660129793853,-1.3875680016887,-5.47938212361419));
#27865=CARTESIAN_POINT('Ctrl Pts',(60.5186445583327,1.38756800168854,-5.47938212361474));
#27866=CARTESIAN_POINT('Ctrl Pts',(61.07127613728,3.82822727268818,-4.15856337748269));
#27867=CARTESIAN_POINT('Ctrl Pts',(61.6239077162275,5.34608279827295,-1.83531254283783));
#27868=CARTESIAN_POINT('Ctrl Pts',(62.1765392951748,5.57525171303254,0.93034496411784));
#27869=CARTESIAN_POINT('Ctrl Pts',(62.7291708741221,4.46049227767768,3.47174049384076));
#27870=CARTESIAN_POINT('Ctrl Pts',(63.2818024530695,2.27052003834545,5.17626430658015));
#27871=CARTESIAN_POINT('Ctrl Pts',(63.8344340320169,-0.466766727102761,
5.63303667998307));
#27872=CARTESIAN_POINT('Ctrl Pts',(64.3870656109642,-3.09153820708416,4.731951492813));
#27873=CARTESIAN_POINT('Ctrl Pts',(64.9396971899116,-4.97108668108975,2.69021757955317));
#27874=CARTESIAN_POINT('Ctrl Pts',(65.492328768859,-5.65234229441848,2.92299128423437E-10));
#27875=CARTESIAN_POINT('Ctrl Pts',(66.0449603478064,-4.97108668146758,-2.69021758030695));
#27876=CARTESIAN_POINT('Ctrl Pts',(66.5975919267537,-3.09153820610978,-4.73195149145368));
#27877=CARTESIAN_POINT('Ctrl Pts',(67.1502235057011,-0.466766729237698,
-5.6330366827348));
#27878=CARTESIAN_POINT('Ctrl Pts',(67.7028550846484,2.27052004287681,-5.17626430084314));
#27879=CARTESIAN_POINT('Ctrl Pts',(68.2554866635959,4.46049226812687,-3.471740505884));
#27880=CARTESIAN_POINT('Ctrl Pts',(68.8081182425432,5.57525173313144,-0.930344938796962));
#27881=CARTESIAN_POINT('Ctrl Pts',(69.3607498214906,5.34608275599143,1.83531248958194));
#27882=CARTESIAN_POINT('Ctrl Pts',(69.9133814004379,3.82822736162757,4.15856348950149));
#27883=CARTESIAN_POINT('Ctrl Pts',(70.4660129793853,1.38756781460721,5.47938188798929));
#27884=CARTESIAN_POINT('Ctrl Pts',(71.0186445583327,-1.38756760817271,5.47938261924127));
#27885=CARTESIAN_POINT('Ctrl Pts',(71.5712761372801,-3.82822810044738,4.15856233495234));
#27886=CARTESIAN_POINT('Ctrl Pts',(72.1239077162274,-5.34608105725119,1.83531473574165));
#27887=CARTESIAN_POINT('Ctrl Pts',(72.6765392951748,-5.57525537632879,-0.930349576908287));
#27888=CARTESIAN_POINT('Ctrl Pts',(73.2291708741222,-4.46048458163846,-3.4717307919688));
#27889=CARTESIAN_POINT('Ctrl Pts',(73.7818024530695,-2.27053630835485,-5.1762847224297));
#27890=CARTESIAN_POINT('Ctrl Pts',(74.3344340320169,0.46680027700503,-5.63299379713529));
#27891=CARTESIAN_POINT('Ctrl Pts',(74.8870656109643,3.09146156820945,-4.73204241007043));
#27892=CARTESIAN_POINT('Ctrl Pts',(75.4396971899116,4.97120383948995,-2.69002843971946));
#27893=CARTESIAN_POINT('Ctrl Pts',(75.8081182425432,5.42478616651165,-0.897005658049129));
#27894=CARTESIAN_POINT('Ctrl Pts',(75.992328768859,5.42478616651165,-7.9721364178528E-15));
#27895=CARTESIAN_POINT('Ctrl Pts',(33.9921997677122,5.49976642738082,0.));
#27896=CARTESIAN_POINT('Ctrl Pts',(34.176410294028,5.49976642738082,0.909403588662882));
#27897=CARTESIAN_POINT('Ctrl Pts',(34.5448313466596,5.03991467318512,2.72720954086847));
#27898=CARTESIAN_POINT('Ctrl Pts',(35.0974629256069,3.13419106663809,4.79744756259311));
#27899=CARTESIAN_POINT('Ctrl Pts',(35.6500945045543,0.473252278446431,5.71085179682633));
#27900=CARTESIAN_POINT('Ctrl Pts',(36.2027260835017,-2.30191914515453,5.24783014539696));
#27901=CARTESIAN_POINT('Ctrl Pts',(36.755357662449,-4.52213639346893,3.51971627798693));
#27902=CARTESIAN_POINT('Ctrl Pts',(37.3079892413964,-5.6523152960574,0.943208655172099));
#27903=CARTESIAN_POINT('Ctrl Pts',(37.8606208203438,-5.41997338236277,-1.86068203981508));
#27904=CARTESIAN_POINT('Ctrl Pts',(38.4132523992911,-3.88114100434969,-4.2160410449643));
#27905=CARTESIAN_POINT('Ctrl Pts',(38.9658839782385,-1.40674625429844,-5.55511740772306));
#27906=CARTESIAN_POINT('Ctrl Pts',(39.5185155571859,1.40674646354598,-5.55511666690852));
#27907=CARTESIAN_POINT('Ctrl Pts',(40.0711471361332,3.88114025546219,-4.21604221461142));
#27908=CARTESIAN_POINT('Ctrl Pts',(40.6237787150806,5.41997510425126,-1.86067976428242));
#27909=CARTESIAN_POINT('Ctrl Pts',(41.1764102940279,5.65231160321522,0.943203956408585));
#27910=CARTESIAN_POINT('Ctrl Pts',(41.7290418729754,4.52214418469897,3.51972611893208));
#27911=CARTESIAN_POINT('Ctrl Pts',(42.2816734519227,2.30190265803137,5.24780945677143));
#27912=CARTESIAN_POINT('Ctrl Pts',(42.8343050308701,-0.473218273533045,
5.71089524334113));
#27913=CARTESIAN_POINT('Ctrl Pts',(43.3869366098174,-3.13426874886167,4.79735545609104));
#27914=CARTESIAN_POINT('Ctrl Pts',(43.9395681887648,-5.03979591868312,2.72740116002078));
#27915=CARTESIAN_POINT('Ctrl Pts',(44.4921997677122,-5.73046769283071,-2.96113953592807E-10));
#27916=CARTESIAN_POINT('Ctrl Pts',(45.0448313466595,-5.03979591830015,-2.72740115925713));
#27917=CARTESIAN_POINT('Ctrl Pts',(45.5974629256069,-3.13426874984933,-4.79735545746814));
#27918=CARTESIAN_POINT('Ctrl Pts',(46.1500945045543,-0.473218271369011,
-5.71089524055342));
#27919=CARTESIAN_POINT('Ctrl Pts',(46.7027260835016,2.30190265343826,-5.24780946258346));
#27920=CARTESIAN_POINT('Ctrl Pts',(47.255357662449,4.52214419437993,-3.51972610673135));
#27921=CARTESIAN_POINT('Ctrl Pts',(47.8079892413964,5.65231158284243,-0.943203982060589));
#27922=CARTESIAN_POINT('Ctrl Pts',(48.3606208203438,5.41997514710894,1.86067981823473));
#27923=CARTESIAN_POINT('Ctrl Pts',(48.9132523992911,3.88114016531086,4.21604210112774));
#27924=CARTESIAN_POINT('Ctrl Pts',(49.4658839782385,1.40674665317661,5.55511690561523));
#27925=CARTESIAN_POINT('Ctrl Pts',(50.0185155571858,-1.40674665317677,5.5551169056147));
#27926=CARTESIAN_POINT('Ctrl Pts',(50.5711471361332,-3.8811401653103,4.2160421011286));
#27927=CARTESIAN_POINT('Ctrl Pts',(51.1237787150806,-5.4199751471102,1.86067981823306));
#27928=CARTESIAN_POINT('Ctrl Pts',(51.676410294028,-5.65231158283973,-0.943203982057156));
#27929=CARTESIAN_POINT('Ctrl Pts',(52.2290418729753,-4.52214419438563,-3.51972610673855));
#27930=CARTESIAN_POINT('Ctrl Pts',(52.7816734519227,-2.30190265342625,-5.24780946256834));
#27931=CARTESIAN_POINT('Ctrl Pts',(53.3343050308701,0.473218271343736,-5.71089524058523));
#27932=CARTESIAN_POINT('Ctrl Pts',(53.8869366098175,3.13426874990249,-4.79735545740122));
#27933=CARTESIAN_POINT('Ctrl Pts',(54.4395681887648,5.0397959181883,-2.72740115939791));
#27934=CARTESIAN_POINT('Ctrl Pts',(54.9921997677122,5.73046769306595,-5.11805824213355E-15));
#27935=CARTESIAN_POINT('Ctrl Pts',(55.5448313466596,5.03979591818831,2.72740115939791));
#27936=CARTESIAN_POINT('Ctrl Pts',(56.0974629256069,3.13426874990249,4.79735545740121));
#27937=CARTESIAN_POINT('Ctrl Pts',(56.6500945045543,0.473218271343732,5.71089524058523));
#27938=CARTESIAN_POINT('Ctrl Pts',(57.2027260835016,-2.30190265342626,5.24780946256833));
#27939=CARTESIAN_POINT('Ctrl Pts',(57.755357662449,-4.52214419438564,3.51972610673854));
#27940=CARTESIAN_POINT('Ctrl Pts',(58.3079892413963,-5.65231158283973,0.943203982057152));
#27941=CARTESIAN_POINT('Ctrl Pts',(58.8606208203438,-5.4199751471102,-1.86067981823306));
#27942=CARTESIAN_POINT('Ctrl Pts',(59.4132523992911,-3.88114016531031,-4.2160421011286));
#27943=CARTESIAN_POINT('Ctrl Pts',(59.9658839782385,-1.40674665317677,-5.55511690561469));
#27944=CARTESIAN_POINT('Ctrl Pts',(60.5185155571859,1.40674665317661,-5.55511690561524));
#27945=CARTESIAN_POINT('Ctrl Pts',(61.0711471361332,3.88114016531085,-4.21604210112775));
#27946=CARTESIAN_POINT('Ctrl Pts',(61.6237787150807,5.41997514710894,-1.86067981823474));
#27947=CARTESIAN_POINT('Ctrl Pts',(62.1764102940279,5.65231158284244,0.943203982060585));
#27948=CARTESIAN_POINT('Ctrl Pts',(62.7290418729753,4.52214419437993,3.51972610673135));
#27949=CARTESIAN_POINT('Ctrl Pts',(63.2816734519227,2.30190265343826,5.24780946258346));
#27950=CARTESIAN_POINT('Ctrl Pts',(63.8343050308701,-0.473218271369009,
5.71089524055341));
#27951=CARTESIAN_POINT('Ctrl Pts',(64.3869366098174,-3.13426874984932,4.79735545746814));
#27952=CARTESIAN_POINT('Ctrl Pts',(64.9395681887648,-5.03979591830014,2.72740115925714));
#27953=CARTESIAN_POINT('Ctrl Pts',(65.4921997677122,-5.73046769283071,2.96121409977839E-10));
#27954=CARTESIAN_POINT('Ctrl Pts',(66.0448313466595,-5.03979591868312,-2.72740116002078));
#27955=CARTESIAN_POINT('Ctrl Pts',(66.5974629256069,-3.13426874886167,-4.79735545609105));
#27956=CARTESIAN_POINT('Ctrl Pts',(67.1500945045543,-0.473218273533038,
-5.71089524334112));
#27957=CARTESIAN_POINT('Ctrl Pts',(67.7027260835016,2.30190265803138,-5.24780945677143));
#27958=CARTESIAN_POINT('Ctrl Pts',(68.255357662449,4.52214418469897,-3.51972611893208));
#27959=CARTESIAN_POINT('Ctrl Pts',(68.8079892413964,5.65231160321522,-0.943203956408587));
#27960=CARTESIAN_POINT('Ctrl Pts',(69.3606208203438,5.41997510425126,1.86067976428242));
#27961=CARTESIAN_POINT('Ctrl Pts',(69.9132523992911,3.88114025546219,4.21604221461142));
#27962=CARTESIAN_POINT('Ctrl Pts',(70.4658839782385,1.40674646354597,5.55511666690853));
#27963=CARTESIAN_POINT('Ctrl Pts',(71.0185155571859,-1.40674625429845,5.55511740772306));
#27964=CARTESIAN_POINT('Ctrl Pts',(71.5711471361332,-3.8811410043497,4.21604104496428));
#27965=CARTESIAN_POINT('Ctrl Pts',(72.1237787150806,-5.41997338236277,1.86068203981508));
#27966=CARTESIAN_POINT('Ctrl Pts',(72.676410294028,-5.65231529605741,-0.943208655172103));
#27967=CARTESIAN_POINT('Ctrl Pts',(73.2290418729754,-4.52213639346892,-3.51971627798694));
#27968=CARTESIAN_POINT('Ctrl Pts',(73.7816734519227,-2.30191914515453,-5.24783014539695));
#27969=CARTESIAN_POINT('Ctrl Pts',(74.3343050308701,0.473252278446422,-5.71085179682633));
#27970=CARTESIAN_POINT('Ctrl Pts',(74.8869366098175,3.13419106663809,-4.79744756259312));
#27971=CARTESIAN_POINT('Ctrl Pts',(75.4395681887648,5.03991467318512,-2.72720954086847));
#27972=CARTESIAN_POINT('Ctrl Pts',(75.8079892413964,5.49976642738082,-0.909403588662883));
#27973=CARTESIAN_POINT('Ctrl Pts',(75.9921997677122,5.49976642738082,-8.08232562162E-15));
#27974=CARTESIAN_POINT('Ctrl Pts',(33.9921997677122,5.49976642738082,5.17361254957654E-35));
#27975=CARTESIAN_POINT('Ctrl Pts',(33.9921996337599,5.49984428540435,5.17361254957654E-35));
#27976=CARTESIAN_POINT('Ctrl Pts',(33.9921994823618,5.49992214302643,0.));
#27977=CARTESIAN_POINT('Ctrl Pts',(33.9921993135185,5.50000000023809,0.));
#27978=CARTESIAN_POINT('Ctrl Pts',(33.9921134030113,5.53961514866854,0.));
#27979=CARTESIAN_POINT('Ctrl Pts',(33.9875106886727,5.57927270787206,0.));
#27980=CARTESIAN_POINT('Ctrl Pts',(33.9693064765724,5.65615401280177,0.));
#27981=CARTESIAN_POINT('Ctrl Pts',(33.955725697793,5.69351111459438,0.));
#27982=CARTESIAN_POINT('Ctrl Pts',(33.9070143140728,5.78787293252881,0.));
#27983=CARTESIAN_POINT('Ctrl Pts',(33.8641799465949,5.84036554141816,0.));
#27984=CARTESIAN_POINT('Ctrl Pts',(33.7655175445174,5.92324377184529,0.));
#27985=CARTESIAN_POINT('Ctrl Pts',(33.7103194075936,5.9548999521189,0.));
#27986=CARTESIAN_POINT('Ctrl Pts',(33.5834982245157,5.99813254826451,0.));
#27987=CARTESIAN_POINT('Ctrl Pts',(33.5193764033541,6.00295356243643,0.));
#27988=CARTESIAN_POINT('Ctrl Pts',(33.3972845623173,5.99470928422369,0.));
#27989=CARTESIAN_POINT('Ctrl Pts',(33.3323414527145,5.97758452130161,0.));
#27990=CARTESIAN_POINT('Ctrl Pts',(33.2112723468849,5.91926289378582,0.));
#27991=CARTESIAN_POINT('Ctrl Pts',(33.1613177334755,5.8799704596013,0.));
#27992=CARTESIAN_POINT('Ctrl Pts',(33.0761471586416,5.78359940593522,0.));
#27993=CARTESIAN_POINT('Ctrl Pts',(33.0420370989278,5.72456593715523,0.));
#27994=CARTESIAN_POINT('Ctrl Pts',(33.0050967455162,5.6177642498931,0.));
#27995=CARTESIAN_POINT('Ctrl Pts',(32.9926516271063,5.56306095689167,-1.33481475863792E-22));
#27996=CARTESIAN_POINT('Ctrl Pts',(32.9926516271063,5.5,-1.33481475863792E-22));
#27997=CARTESIAN_POINT('Ctrl Pts',(75.9921997677122,5.49976642738082,-8.88178419700125E-15));
#27998=CARTESIAN_POINT('Ctrl Pts',(75.99219963376,5.49984428532499,-8.88189861517979E-15));
#27999=CARTESIAN_POINT('Ctrl Pts',(75.9921994823621,5.4999221428677,-8.88203003829887E-15));
#28000=CARTESIAN_POINT('Ctrl Pts',(75.992199313519,5.5,-8.88214445528432E-15));
#28001=CARTESIAN_POINT('Ctrl Pts',(75.9921134030299,5.53961514843935,-8.94036193296511E-15));
#28002=CARTESIAN_POINT('Ctrl Pts',(75.9875106887073,5.57927270765391,-9.00722814171805E-15));
#28003=CARTESIAN_POINT('Ctrl Pts',(75.9693064766338,5.65615401261384,-9.1202110745582E-15));
#28004=CARTESIAN_POINT('Ctrl Pts',(75.955725697865,5.69351111442127,-8.84808572513712E-15));
#28005=CARTESIAN_POINT('Ctrl Pts',(75.9070143141801,5.78787293237739,-8.98675760312315E-15));
#28006=CARTESIAN_POINT('Ctrl Pts',(75.8641799467243,5.84036554127547,-9.07499142441514E-15));
#28007=CARTESIAN_POINT('Ctrl Pts',(75.7655175446779,5.92324377174254,-9.19678729600774E-15));
#28008=CARTESIAN_POINT('Ctrl Pts',(75.7103194077563,5.95489995203899,-9.24849061649267E-15));
#28009=CARTESIAN_POINT('Ctrl Pts',(75.583498224688,5.99813254823382,-9.31202420915126E-15));
#28010=CARTESIAN_POINT('Ctrl Pts',(75.5193764035373,6.00295356242793,-9.45958558899066E-15));
#28011=CARTESIAN_POINT('Ctrl Pts',(75.3972845624903,5.99470928425966,-9.4474699943466E-15));
#28012=CARTESIAN_POINT('Ctrl Pts',(75.3323414528765,5.9775845213551,-9.4182367933636E-15));
#28013=CARTESIAN_POINT('Ctrl Pts',(75.2112723471179,5.91926289392378,-9.3325287201378E-15));
#28014=CARTESIAN_POINT('Ctrl Pts',(75.1613177336804,5.879970459797,-9.41550176458032E-15));
#28015=CARTESIAN_POINT('Ctrl Pts',(75.0761471587424,5.78359940608845,-9.27387716163476E-15));
#28016=CARTESIAN_POINT('Ctrl Pts',(75.0420370990085,5.72456593731634,-9.17263343837334E-15));
#28017=CARTESIAN_POINT('Ctrl Pts',(75.005096745547,5.61776425003271,-9.01568022500282E-15));
#28018=CARTESIAN_POINT('Ctrl Pts',(74.9926516271063,5.56306095696798,-8.97445707592366E-15));
#28019=CARTESIAN_POINT('Ctrl Pts',(74.9926516271063,5.5,-8.88178419700125E-15));
#28020=CARTESIAN_POINT('Origin',(75.4926516271063,5.5,-8.08266887437253E-15));
#28021=CARTESIAN_POINT('Origin',(33.4926516271063,5.5,0.));
#28022=CARTESIAN_POINT('',(0.,0.,0.));
#28023=CARTESIAN_POINT('',(0.,0.,0.));
#28024=CARTESIAN_POINT('',(0.,0.,0.));
#28025=CARTESIAN_POINT('',(0.,0.,0.));
#28026=CARTESIAN_POINT('',(0.,0.,0.));
#28027=CARTESIAN_POINT('',(0.,0.,0.));
#28028=CARTESIAN_POINT('',(0.,0.,0.));
#28029=CARTESIAN_POINT('',(0.,0.,0.));
#28030=CARTESIAN_POINT('',(0.,0.,0.));
#28031=CARTESIAN_POINT('',(0.,0.,0.));
#28032=UNCERTAINTY_MEASURE_WITH_UNIT(LENGTH_MEASURE(0.01),#28056,
'DISTANCE_ACCURACY_VALUE',
'Maximum model space distance between geometric entities at asserted c
onnectivities');
#28033=UNCERTAINTY_MEASURE_WITH_UNIT(LENGTH_MEASURE(0.01),#28056,
'DISTANCE_ACCURACY_VALUE',
'Maximum model space distance between geometric entities at asserted c
onnectivities');
#28034=UNCERTAINTY_MEASURE_WITH_UNIT(LENGTH_MEASURE(0.01),#28056,
'DISTANCE_ACCURACY_VALUE',
'Maximum model space distance between geometric entities at asserted c
onnectivities');
#28035=UNCERTAINTY_MEASURE_WITH_UNIT(LENGTH_MEASURE(0.01),#28056,
'DISTANCE_ACCURACY_VALUE',
'Maximum model space distance between geometric entities at asserted c
onnectivities');
#28036=UNCERTAINTY_MEASURE_WITH_UNIT(LENGTH_MEASURE(0.01),#28056,
'DISTANCE_ACCURACY_VALUE',
'Maximum model space distance between geometric entities at asserted c
onnectivities');
#28037=UNCERTAINTY_MEASURE_WITH_UNIT(LENGTH_MEASURE(0.01),#28056,
'DISTANCE_ACCURACY_VALUE',
'Maximum model space distance between geometric entities at asserted c
onnectivities');
#28038=UNCERTAINTY_MEASURE_WITH_UNIT(LENGTH_MEASURE(0.01),#28056,
'DISTANCE_ACCURACY_VALUE',
'Maximum model space distance between geometric entities at asserted c
onnectivities');
#28039=UNCERTAINTY_MEASURE_WITH_UNIT(LENGTH_MEASURE(0.01),#28056,
'DISTANCE_ACCURACY_VALUE',
'Maximum model space distance between geometric entities at asserted c
onnectivities');
#28040=UNCERTAINTY_MEASURE_WITH_UNIT(LENGTH_MEASURE(0.01),#28056,
'DISTANCE_ACCURACY_VALUE',
'Maximum model space distance between geometric entities at asserted c
onnectivities');
#28041=UNCERTAINTY_MEASURE_WITH_UNIT(LENGTH_MEASURE(0.01),#28056,
'DISTANCE_ACCURACY_VALUE',
'Maximum model space distance between geometric entities at asserted c
onnectivities');
#28042=UNCERTAINTY_MEASURE_WITH_UNIT(LENGTH_MEASURE(0.01),#28056,
'DISTANCE_ACCURACY_VALUE',
'Maximum model space distance between geometric entities at asserted c
onnectivities');
#28043=UNCERTAINTY_MEASURE_WITH_UNIT(LENGTH_MEASURE(0.01),#28056,
'DISTANCE_ACCURACY_VALUE',
'Maximum model space distance between geometric entities at asserted c
onnectivities');
#28044=(
GEOMETRIC_REPRESENTATION_CONTEXT(3)
GLOBAL_UNCERTAINTY_ASSIGNED_CONTEXT((#28032))
GLOBAL_UNIT_ASSIGNED_CONTEXT((#28056,#28058,#28059))
REPRESENTATION_CONTEXT('','3D')
);
#28045=(
GEOMETRIC_REPRESENTATION_CONTEXT(3)
GLOBAL_UNCERTAINTY_ASSIGNED_CONTEXT((#28033))
GLOBAL_UNIT_ASSIGNED_CONTEXT((#28056,#28058,#28059))
REPRESENTATION_CONTEXT('','3D')
);
#28046=(
GEOMETRIC_REPRESENTATION_CONTEXT(3)
GLOBAL_UNCERTAINTY_ASSIGNED_CONTEXT((#28034))
GLOBAL_UNIT_ASSIGNED_CONTEXT((#28056,#28058,#28059))
REPRESENTATION_CONTEXT('','3D')
);
#28047=(
GEOMETRIC_REPRESENTATION_CONTEXT(3)
GLOBAL_UNCERTAINTY_ASSIGNED_CONTEXT((#28035))
GLOBAL_UNIT_ASSIGNED_CONTEXT((#28056,#28058,#28059))
REPRESENTATION_CONTEXT('','3D')
);
#28048=(
GEOMETRIC_REPRESENTATION_CONTEXT(3)
GLOBAL_UNCERTAINTY_ASSIGNED_CONTEXT((#28036))
GLOBAL_UNIT_ASSIGNED_CONTEXT((#28056,#28058,#28059))
REPRESENTATION_CONTEXT('','3D')
);
#28049=(
GEOMETRIC_REPRESENTATION_CONTEXT(3)
GLOBAL_UNCERTAINTY_ASSIGNED_CONTEXT((#28037))
GLOBAL_UNIT_ASSIGNED_CONTEXT((#28056,#28058,#28059))
REPRESENTATION_CONTEXT('','3D')
);
#28050=(
GEOMETRIC_REPRESENTATION_CONTEXT(3)
GLOBAL_UNCERTAINTY_ASSIGNED_CONTEXT((#28038))
GLOBAL_UNIT_ASSIGNED_CONTEXT((#28056,#28058,#28059))
REPRESENTATION_CONTEXT('','3D')
);
#28051=(
GEOMETRIC_REPRESENTATION_CONTEXT(3)
GLOBAL_UNCERTAINTY_ASSIGNED_CONTEXT((#28039))
GLOBAL_UNIT_ASSIGNED_CONTEXT((#28056,#28058,#28059))
REPRESENTATION_CONTEXT('','3D')
);
#28052=(
GEOMETRIC_REPRESENTATION_CONTEXT(3)
GLOBAL_UNCERTAINTY_ASSIGNED_CONTEXT((#28040))
GLOBAL_UNIT_ASSIGNED_CONTEXT((#28056,#28058,#28059))
REPRESENTATION_CONTEXT('','3D')
);
#28053=(
GEOMETRIC_REPRESENTATION_CONTEXT(3)
GLOBAL_UNCERTAINTY_ASSIGNED_CONTEXT((#28041))
GLOBAL_UNIT_ASSIGNED_CONTEXT((#28056,#28058,#28059))
REPRESENTATION_CONTEXT('','3D')
);
#28054=(
GEOMETRIC_REPRESENTATION_CONTEXT(3)
GLOBAL_UNCERTAINTY_ASSIGNED_CONTEXT((#28042))
GLOBAL_UNIT_ASSIGNED_CONTEXT((#28056,#28058,#28059))
REPRESENTATION_CONTEXT('','3D')
);
#28055=(
GEOMETRIC_REPRESENTATION_CONTEXT(3)
GLOBAL_UNCERTAINTY_ASSIGNED_CONTEXT((#28043))
GLOBAL_UNIT_ASSIGNED_CONTEXT((#28056,#28058,#28059))
REPRESENTATION_CONTEXT('','3D')
);
#28056=(
LENGTH_UNIT()
NAMED_UNIT(*)
SI_UNIT(.MILLI.,.METRE.)
);
#28057=(
LENGTH_UNIT()
NAMED_UNIT(*)
SI_UNIT($,.METRE.)
);
#28058=(
NAMED_UNIT(*)
PLANE_ANGLE_UNIT()
SI_UNIT($,.RADIAN.)
);
#28059=(
NAMED_UNIT(*)
SI_UNIT($,.STERADIAN.)
SOLID_ANGLE_UNIT()
);
#28060=SHAPE_DEFINITION_REPRESENTATION(#28071,#28092);
#28061=SHAPE_DEFINITION_REPRESENTATION(#28072,#28093);
#28062=SHAPE_DEFINITION_REPRESENTATION(#28073,#28094);
#28063=SHAPE_DEFINITION_REPRESENTATION(#28074,#28095);
#28064=SHAPE_DEFINITION_REPRESENTATION(#28075,#28096);
#28065=SHAPE_DEFINITION_REPRESENTATION(#28076,#28097);
#28066=SHAPE_DEFINITION_REPRESENTATION(#28077,#28098);
#28067=SHAPE_DEFINITION_REPRESENTATION(#28078,#28099);
#28068=SHAPE_DEFINITION_REPRESENTATION(#28079,#28100);
#28069=SHAPE_DEFINITION_REPRESENTATION(#28080,#28101);
#28070=SHAPE_DEFINITION_REPRESENTATION(#28081,#28102);
#28071=PRODUCT_DEFINITION_SHAPE('',$,#28104);
#28072=PRODUCT_DEFINITION_SHAPE('',$,#28105);
#28073=PRODUCT_DEFINITION_SHAPE('',$,#28106);
#28074=PRODUCT_DEFINITION_SHAPE('',$,#28107);
#28075=PRODUCT_DEFINITION_SHAPE('',$,#28108);
#28076=PRODUCT_DEFINITION_SHAPE('',$,#28109);
#28077=PRODUCT_DEFINITION_SHAPE('',$,#28110);
#28078=PRODUCT_DEFINITION_SHAPE('',$,#28111);
#28079=PRODUCT_DEFINITION_SHAPE('',$,#28112);
#28080=PRODUCT_DEFINITION_SHAPE('',$,#28113);
#28081=PRODUCT_DEFINITION_SHAPE('',$,#28114);
#28082=PRODUCT_DEFINITION_SHAPE($,$,#41);
#28083=PRODUCT_DEFINITION_SHAPE($,$,#42);
#28084=PRODUCT_DEFINITION_SHAPE($,$,#43);
#28085=PRODUCT_DEFINITION_SHAPE($,$,#44);
#28086=PRODUCT_DEFINITION_SHAPE($,$,#45);
#28087=PRODUCT_DEFINITION_SHAPE($,$,#46);
#28088=PRODUCT_DEFINITION_SHAPE($,$,#47);
#28089=PRODUCT_DEFINITION_SHAPE($,$,#48);
#28090=PRODUCT_DEFINITION_SHAPE($,$,#49);
#28091=PRODUCT_DEFINITION_SHAPE($,$,#50);
#28092=SHAPE_REPRESENTATION('',(#3800,#4104,#4105,#4106,#4107,#4108,#4109,
#4110,#4111,#4112,#4113),#28044);
#28093=SHAPE_REPRESENTATION('',(#3801),#28045);
#28094=SHAPE_REPRESENTATION('',(#3851),#28046);
#28095=SHAPE_REPRESENTATION('',(#3947),#28047);
#28096=SHAPE_REPRESENTATION('',(#3962),#28048);
#28097=SHAPE_REPRESENTATION('',(#3990),#28049);
#28098=SHAPE_REPRESENTATION('',(#4002),#28050);
#28099=SHAPE_REPRESENTATION('',(#4014),#28051);
#28100=SHAPE_REPRESENTATION('',(#4059),#28052);
#28101=SHAPE_REPRESENTATION('',(#4086),#28053);
#28102=SHAPE_REPRESENTATION('',(#4101),#28054);
#28103=PRODUCT_DEFINITION_CONTEXT('part definition',#28138,'design');
#28104=PRODUCT_DEFINITION('BR-313','BR-313',#28115,#28103);
#28105=PRODUCT_DEFINITION('Cylinder','Cylinder',#28116,#28103);
#28106=PRODUCT_DEFINITION('Shaft','Shaft',#28117,#28103);
#28107=PRODUCT_DEFINITION('Nut_02','Nut_02',#28118,#28103);
#28108=PRODUCT_DEFINITION('Screw','Screw',#28119,#28103);
#28109=PRODUCT_DEFINITION('Ring_02','Ring_02',#28120,#28103);
#28110=PRODUCT_DEFINITION('Ring_01','Ring_01',#28121,#28103);
#28111=PRODUCT_DEFINITION('Screw_02','Screw_02',#28122,#28103);
#28112=PRODUCT_DEFINITION('spacer','Spacer',#28123,#28103);
#28113=PRODUCT_DEFINITION('Nut_01','Nut_01',#28124,#28103);
#28114=PRODUCT_DEFINITION('Spring','Spring',#28125,#28103);
#28115=PRODUCT_DEFINITION_FORMATION('',$,#28140);
#28116=PRODUCT_DEFINITION_FORMATION('',$,#28141);
#28117=PRODUCT_DEFINITION_FORMATION('',$,#28142);
#28118=PRODUCT_DEFINITION_FORMATION('',$,#28143);
#28119=PRODUCT_DEFINITION_FORMATION('',$,#28144);
#28120=PRODUCT_DEFINITION_FORMATION('',$,#28145);
#28121=PRODUCT_DEFINITION_FORMATION('',$,#28146);
#28122=PRODUCT_DEFINITION_FORMATION('',$,#28147);
#28123=PRODUCT_DEFINITION_FORMATION('',$,#28148);
#28124=PRODUCT_DEFINITION_FORMATION('',$,#28149);
#28125=PRODUCT_DEFINITION_FORMATION('',$,#28150);
#28126=PRODUCT_RELATED_PRODUCT_CATEGORY('BR-313','BR-313',(#28140));
#28127=PRODUCT_RELATED_PRODUCT_CATEGORY('Cylinder','Cylinder',(#28141));
#28128=PRODUCT_RELATED_PRODUCT_CATEGORY('Shaft','Shaft',(#28142));
#28129=PRODUCT_RELATED_PRODUCT_CATEGORY('Nut_02','Nut_02',(#28143));
#28130=PRODUCT_RELATED_PRODUCT_CATEGORY('Screw','Screw',(#28144));
#28131=PRODUCT_RELATED_PRODUCT_CATEGORY('Ring_02','Ring_02',(#28145));
#28132=PRODUCT_RELATED_PRODUCT_CATEGORY('Ring_01','Ring_01',(#28146));
#28133=PRODUCT_RELATED_PRODUCT_CATEGORY('Screw_02','Screw_02',(#28147));
#28134=PRODUCT_RELATED_PRODUCT_CATEGORY('Spacer','Spacer',(#28148));
#28135=PRODUCT_RELATED_PRODUCT_CATEGORY('Nut_01','Nut_01',(#28149));
#28136=PRODUCT_RELATED_PRODUCT_CATEGORY('Spring','Spring',(#28150));
#28137=APPLICATION_PROTOCOL_DEFINITION('international standard',
'automotive_design',2009,#28138);
#28138=APPLICATION_CONTEXT(
'Core Data for Automotive Mechanical Design Process');
#28139=PRODUCT_CONTEXT('part definition',#28138,'mechanical');
#28140=PRODUCT('BR-313','BR-313',$,(#28139));
#28141=PRODUCT('Cylinder','Cylinder',$,(#28139));
#28142=PRODUCT('Shaft','Shaft',$,(#28139));
#28143=PRODUCT('Nut_02','Nut_02',$,(#28139));
#28144=PRODUCT('Screw','Screw',$,(#28139));
#28145=PRODUCT('Ring_02','Ring_02',$,(#28139));
#28146=PRODUCT('Ring_01','Ring_01',$,(#28139));
#28147=PRODUCT('Screw_02','Screw_02',$,(#28139));
#28148=PRODUCT('spacer','Spacer',$,(#28139));
#28149=PRODUCT('Nut_01','Nut_01',$,(#28139));
#28150=PRODUCT('Spring','Spring',$,(#28139));
#28151=PRESENTATION_STYLE_ASSIGNMENT((#28154));
#28152=PRESENTATION_STYLE_ASSIGNMENT((#28155));
#28153=PRESENTATION_STYLE_ASSIGNMENT((#28156));
#28154=SURFACE_STYLE_USAGE(.BOTH.,#28157);
#28155=SURFACE_STYLE_USAGE(.BOTH.,#28158);
#28156=SURFACE_STYLE_USAGE(.BOTH.,#28159);
#28157=SURFACE_SIDE_STYLE('',(#28160));
#28158=SURFACE_SIDE_STYLE('',(#28161));
#28159=SURFACE_SIDE_STYLE('',(#28162));
#28160=SURFACE_STYLE_FILL_AREA(#28163);
#28161=SURFACE_STYLE_FILL_AREA(#28164);
#28162=SURFACE_STYLE_FILL_AREA(#28165);
#28163=FILL_AREA_STYLE('Steel - Satin',(#28166));
#28164=FILL_AREA_STYLE('Opaque(160,160,160)',(#28167));
#28165=FILL_AREA_STYLE('Opaque(39,39,39)',(#28168));
#28166=FILL_AREA_STYLE_COLOUR('Steel - Satin',#28169);
#28167=FILL_AREA_STYLE_COLOUR('Opaque(160,160,160)',#28170);
#28168=FILL_AREA_STYLE_COLOUR('Opaque(39,39,39)',#28171);
#28169=COLOUR_RGB('Steel - Satin', 0.09019608, 0.27058824, 0.51372549);
#28170=COLOUR_RGB('Opaque(160,160,160)', 0.66274510, 0.83137255, 0.94901961);
#28171=COLOUR_RGB('Opaque(39,39,39)', 0.08235294, 0.09019608, 0.10196078);
ENDSEC;
END-ISO-10303-21;
